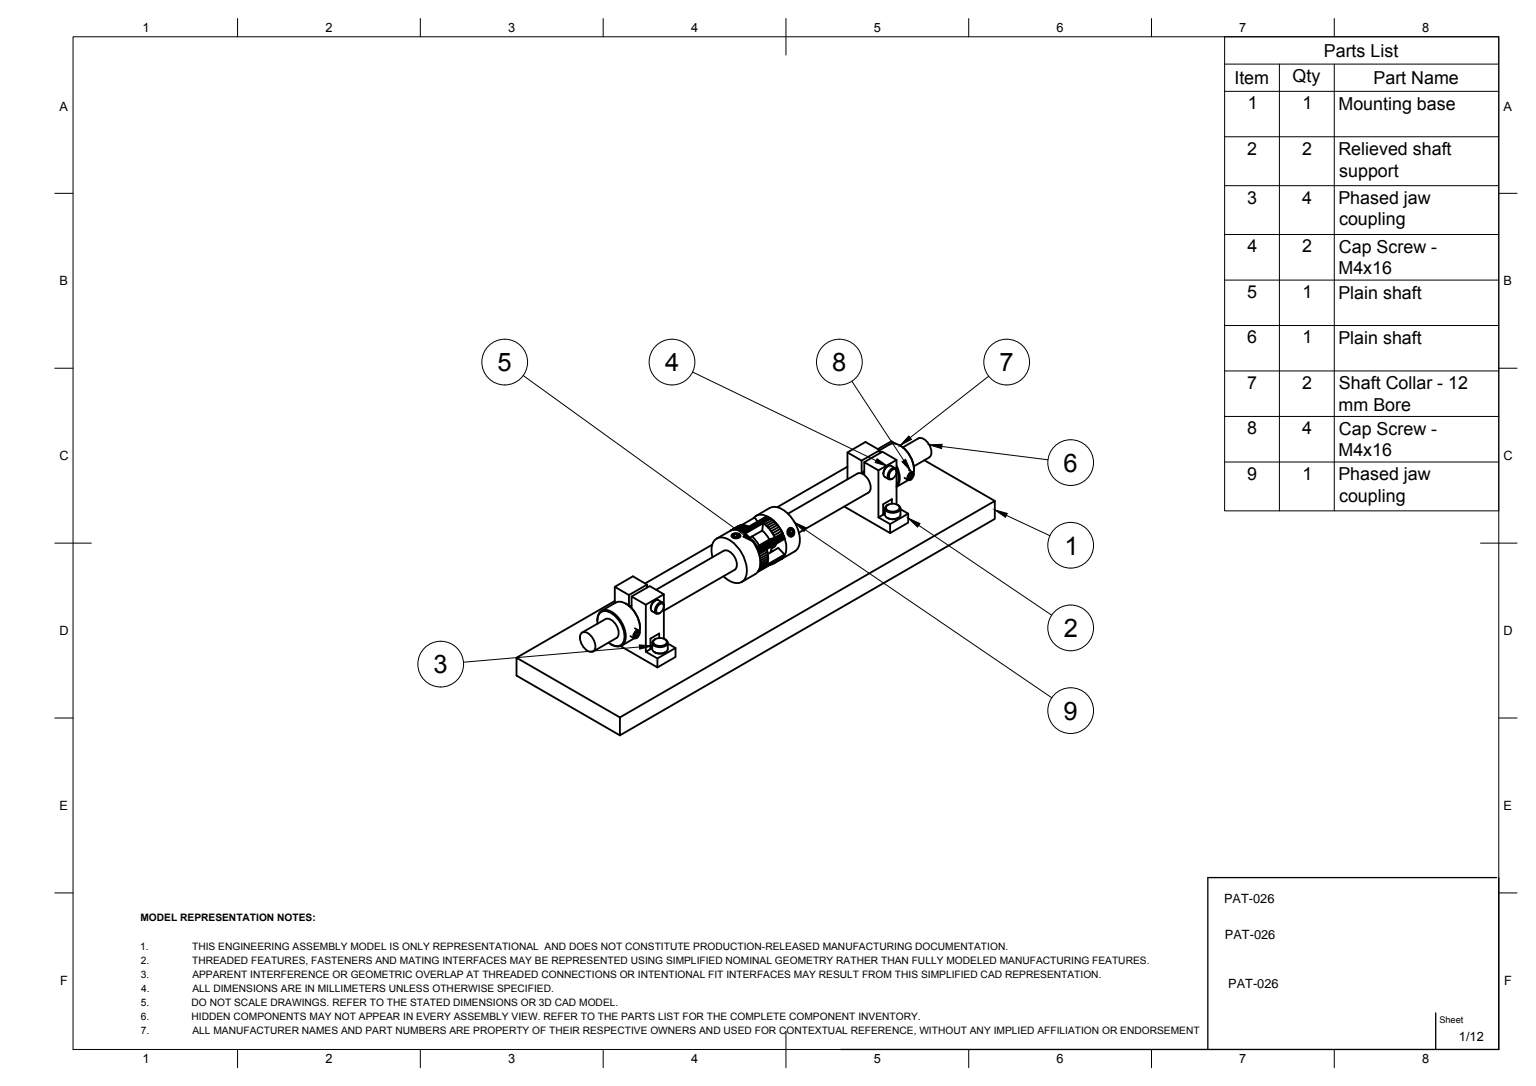
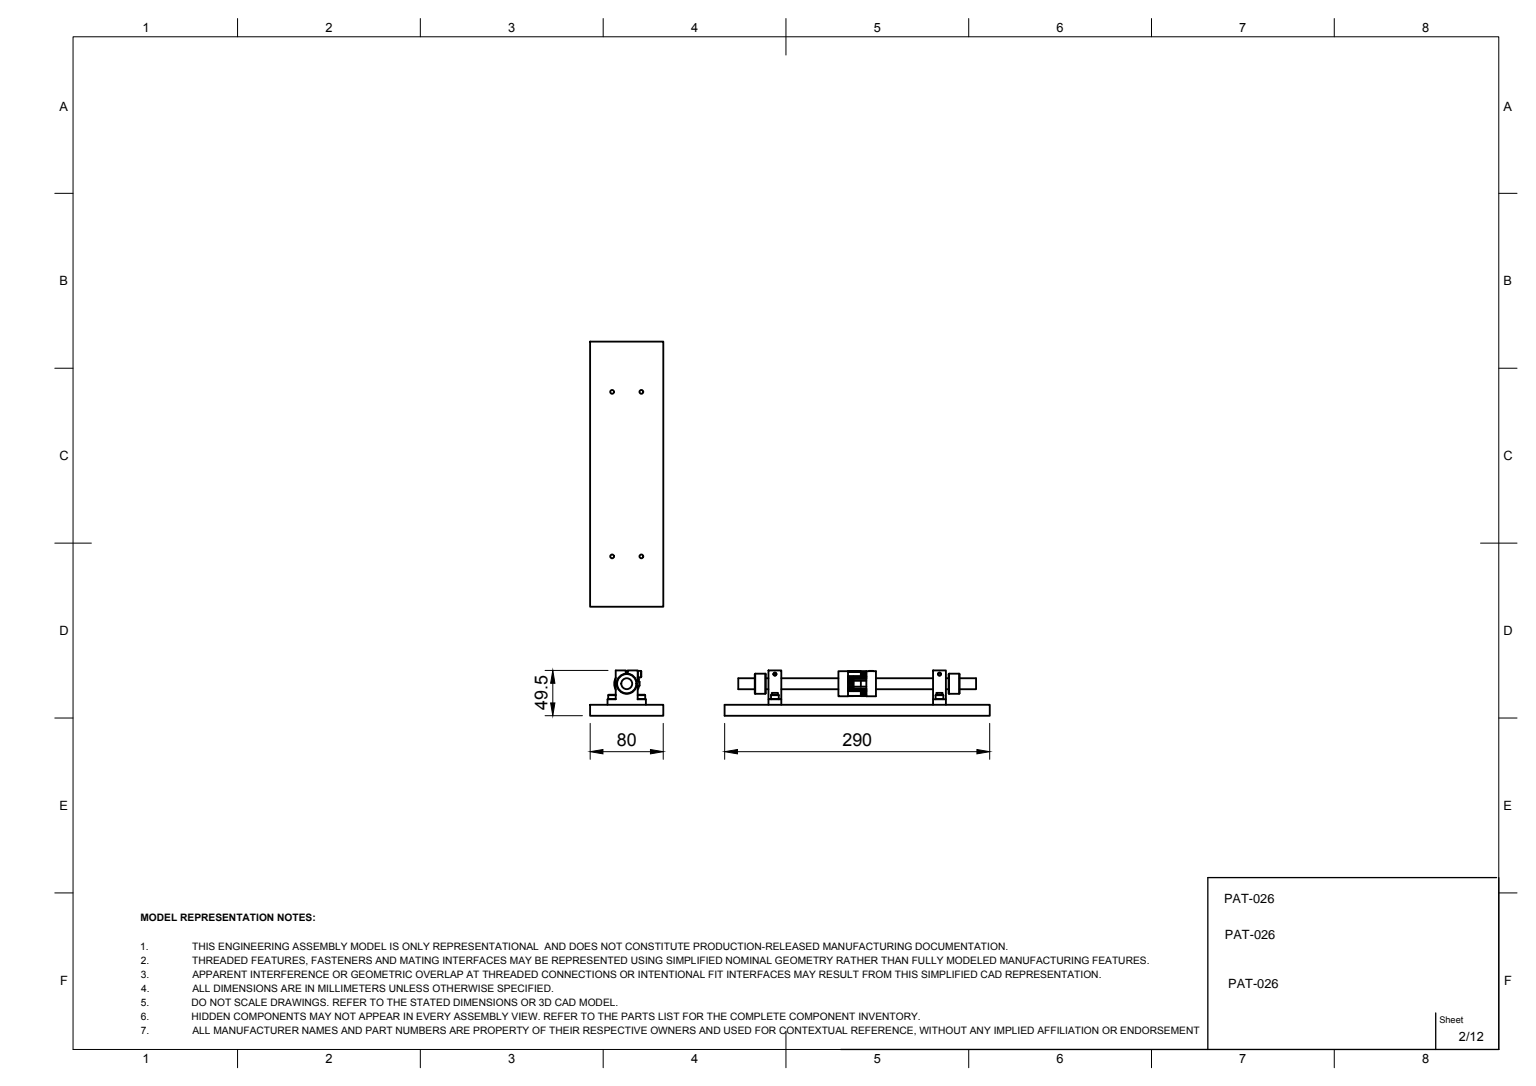
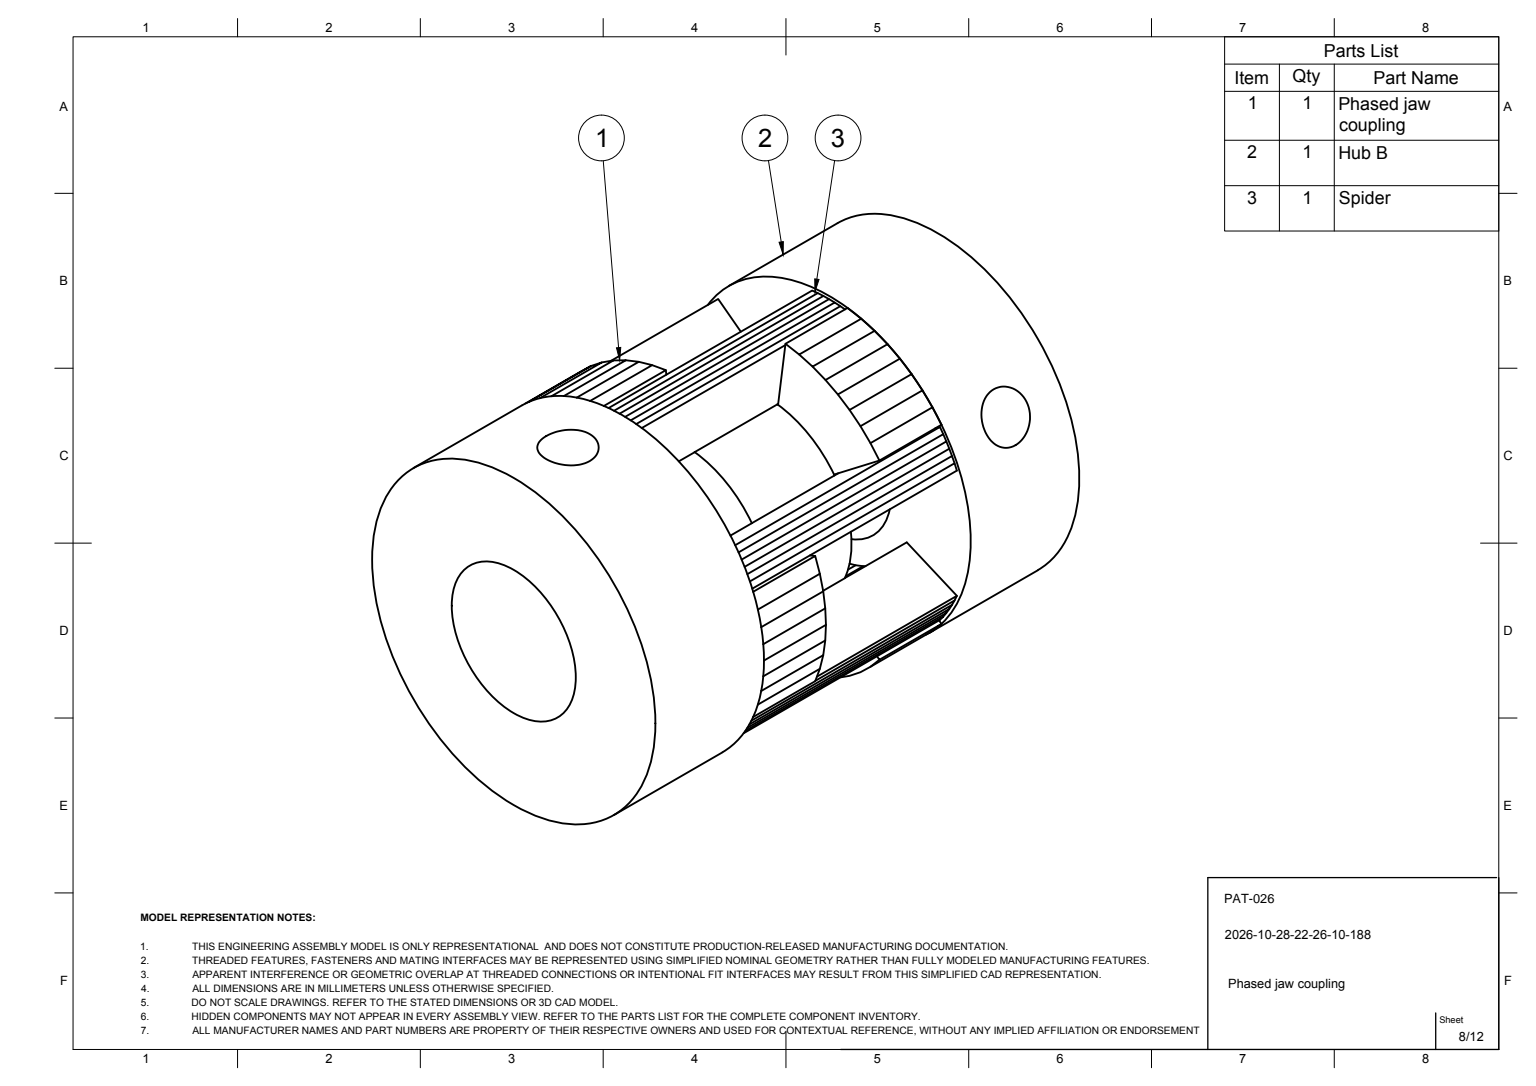
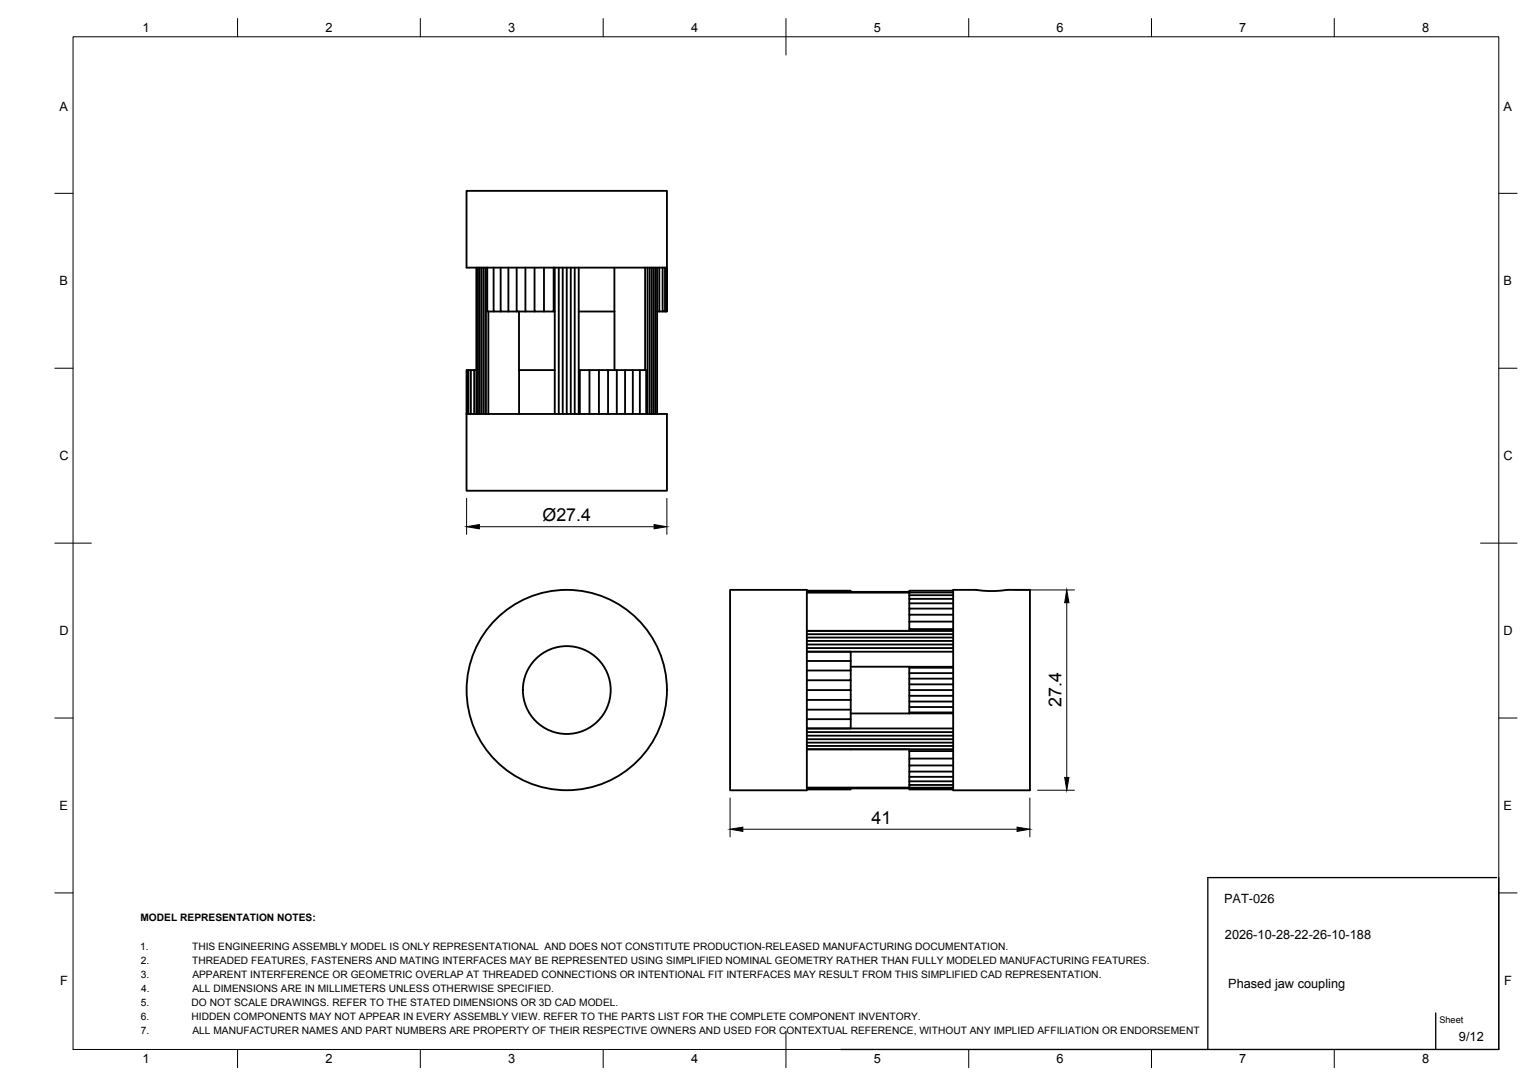
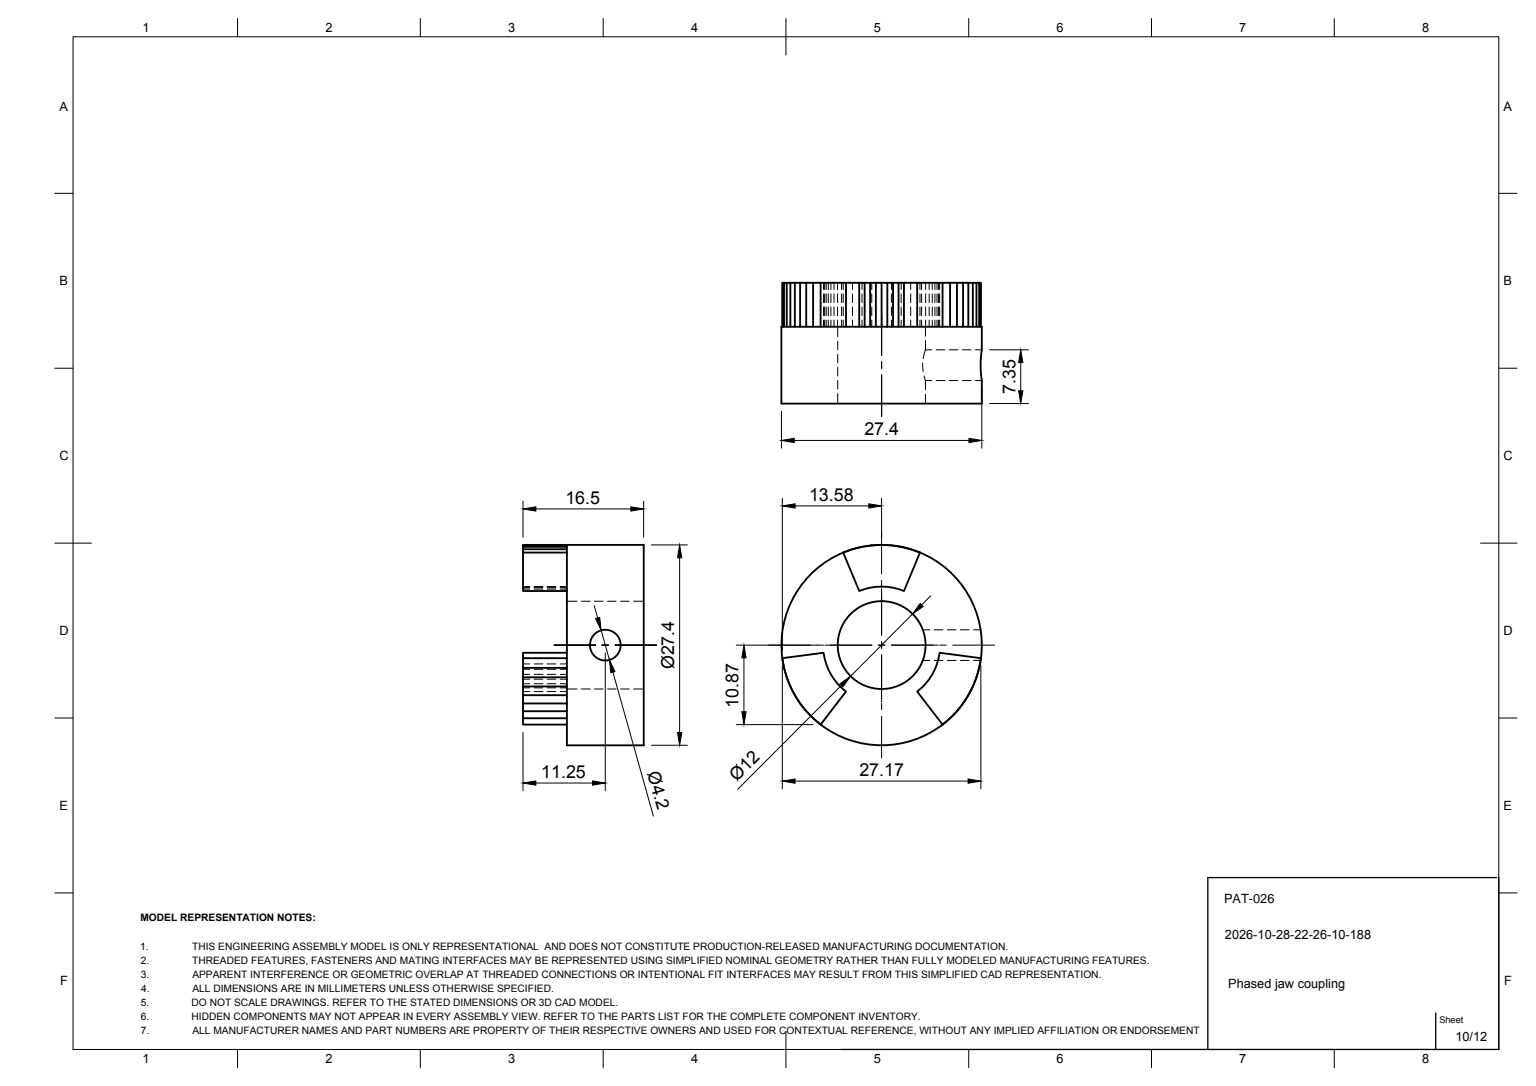
ISO-10303-21;
HEADER;
/* Generated by software containing ST-Developer
 * from STEP Tools, Inc. (www.steptools.com) 
 */

FILE_DESCRIPTION(
/* description */ ('PAT-026'),
/* implementation_level */ '2;1');

FILE_NAME(
/* name */ 'PAT-026',
/* time_stamp */ '2026-10-28T22:25:58-07:00',
/* author */ (''),
/* organization */ (''),
/* preprocessor_version */ 'ST-DEVELOPER v20.2',
/* originating_system */ 'Autodesk Translation Framework v15.17.0.0',
/* authorisation */ '');

FILE_SCHEMA (('AUTOMOTIVE_DESIGN { 1 0 10303 214 3 1 1 }'));
ENDSEC;

DATA;
#10=MECHANICAL_DESIGN_GEOMETRIC_PRESENTATION_REPRESENTATION('',(#141,#142,
#143,#144,#145,#146,#147,#148,#149,#150,#151),#12343);
#11=ITEM_DEFINED_TRANSFORMATION($,$,#7617,#8006);
#12=ITEM_DEFINED_TRANSFORMATION($,$,#7735,#8007);
#13=ITEM_DEFINED_TRANSFORMATION($,$,#7853,#8008);
#14=ITEM_DEFINED_TRANSFORMATION($,$,#7483,#8026);
#15=ITEM_DEFINED_TRANSFORMATION($,$,#7502,#8027);
#16=ITEM_DEFINED_TRANSFORMATION($,$,#7508,#8028);
#17=ITEM_DEFINED_TRANSFORMATION($,$,#7514,#8029);
#18=ITEM_DEFINED_TRANSFORMATION($,$,#7552,#8030);
#19=ITEM_DEFINED_TRANSFORMATION($,$,#7552,#8031);
#20=ITEM_DEFINED_TRANSFORMATION($,$,#7576,#8032);
#21=ITEM_DEFINED_TRANSFORMATION($,$,#7514,#8033);
#22=ITEM_DEFINED_TRANSFORMATION($,$,#7552,#8034);
#23=ITEM_DEFINED_TRANSFORMATION($,$,#7552,#8035);
#24=ITEM_DEFINED_TRANSFORMATION($,$,#7576,#8036);
#25=ITEM_DEFINED_TRANSFORMATION($,$,#7602,#8037);
#26=ITEM_DEFINED_TRANSFORMATION($,$,#8009,#8038);
#27=ITEM_DEFINED_TRANSFORMATION($,$,#7602,#8039);
#28=ITEM_DEFINED_TRANSFORMATION($,$,#8009,#8040);
#29=ITEM_DEFINED_TRANSFORMATION($,$,#7616,#8041);
#30=ITEM_DEFINED_TRANSFORMATION($,$,#8009,#8042);
#31=ITEM_DEFINED_TRANSFORMATION($,$,#8009,#8043);
#32=(
REPRESENTATION_RELATIONSHIP($,$,#12404,#12403)
REPRESENTATION_RELATIONSHIP_WITH_TRANSFORMATION(#11)
SHAPE_REPRESENTATION_RELATIONSHIP()
);
#33=(
REPRESENTATION_RELATIONSHIP($,$,#12405,#12403)
REPRESENTATION_RELATIONSHIP_WITH_TRANSFORMATION(#12)
SHAPE_REPRESENTATION_RELATIONSHIP()
);
#34=(
REPRESENTATION_RELATIONSHIP($,$,#12406,#12403)
REPRESENTATION_RELATIONSHIP_WITH_TRANSFORMATION(#13)
SHAPE_REPRESENTATION_RELATIONSHIP()
);
#35=(
REPRESENTATION_RELATIONSHIP($,$,#12396,#12395)
REPRESENTATION_RELATIONSHIP_WITH_TRANSFORMATION(#14)
SHAPE_REPRESENTATION_RELATIONSHIP()
);
#36=(
REPRESENTATION_RELATIONSHIP($,$,#12397,#12395)
REPRESENTATION_RELATIONSHIP_WITH_TRANSFORMATION(#15)
SHAPE_REPRESENTATION_RELATIONSHIP()
);
#37=(
REPRESENTATION_RELATIONSHIP($,$,#12398,#12395)
REPRESENTATION_RELATIONSHIP_WITH_TRANSFORMATION(#16)
SHAPE_REPRESENTATION_RELATIONSHIP()
);
#38=(
REPRESENTATION_RELATIONSHIP($,$,#12399,#12395)
REPRESENTATION_RELATIONSHIP_WITH_TRANSFORMATION(#17)
SHAPE_REPRESENTATION_RELATIONSHIP()
);
#39=(
REPRESENTATION_RELATIONSHIP($,$,#12400,#12395)
REPRESENTATION_RELATIONSHIP_WITH_TRANSFORMATION(#18)
SHAPE_REPRESENTATION_RELATIONSHIP()
);
#40=(
REPRESENTATION_RELATIONSHIP($,$,#12400,#12395)
REPRESENTATION_RELATIONSHIP_WITH_TRANSFORMATION(#19)
SHAPE_REPRESENTATION_RELATIONSHIP()
);
#41=(
REPRESENTATION_RELATIONSHIP($,$,#12401,#12395)
REPRESENTATION_RELATIONSHIP_WITH_TRANSFORMATION(#20)
SHAPE_REPRESENTATION_RELATIONSHIP()
);
#42=(
REPRESENTATION_RELATIONSHIP($,$,#12399,#12395)
REPRESENTATION_RELATIONSHIP_WITH_TRANSFORMATION(#21)
SHAPE_REPRESENTATION_RELATIONSHIP()
);
#43=(
REPRESENTATION_RELATIONSHIP($,$,#12400,#12395)
REPRESENTATION_RELATIONSHIP_WITH_TRANSFORMATION(#22)
SHAPE_REPRESENTATION_RELATIONSHIP()
);
#44=(
REPRESENTATION_RELATIONSHIP($,$,#12400,#12395)
REPRESENTATION_RELATIONSHIP_WITH_TRANSFORMATION(#23)
SHAPE_REPRESENTATION_RELATIONSHIP()
);
#45=(
REPRESENTATION_RELATIONSHIP($,$,#12401,#12395)
REPRESENTATION_RELATIONSHIP_WITH_TRANSFORMATION(#24)
SHAPE_REPRESENTATION_RELATIONSHIP()
);
#46=(
REPRESENTATION_RELATIONSHIP($,$,#12402,#12395)
REPRESENTATION_RELATIONSHIP_WITH_TRANSFORMATION(#25)
SHAPE_REPRESENTATION_RELATIONSHIP()
);
#47=(
REPRESENTATION_RELATIONSHIP($,$,#12407,#12395)
REPRESENTATION_RELATIONSHIP_WITH_TRANSFORMATION(#26)
SHAPE_REPRESENTATION_RELATIONSHIP()
);
#48=(
REPRESENTATION_RELATIONSHIP($,$,#12402,#12395)
REPRESENTATION_RELATIONSHIP_WITH_TRANSFORMATION(#27)
SHAPE_REPRESENTATION_RELATIONSHIP()
);
#49=(
REPRESENTATION_RELATIONSHIP($,$,#12407,#12395)
REPRESENTATION_RELATIONSHIP_WITH_TRANSFORMATION(#28)
SHAPE_REPRESENTATION_RELATIONSHIP()
);
#50=(
REPRESENTATION_RELATIONSHIP($,$,#12403,#12395)
REPRESENTATION_RELATIONSHIP_WITH_TRANSFORMATION(#29)
SHAPE_REPRESENTATION_RELATIONSHIP()
);
#51=(
REPRESENTATION_RELATIONSHIP($,$,#12407,#12395)
REPRESENTATION_RELATIONSHIP_WITH_TRANSFORMATION(#30)
SHAPE_REPRESENTATION_RELATIONSHIP()
);
#52=(
REPRESENTATION_RELATIONSHIP($,$,#12407,#12395)
REPRESENTATION_RELATIONSHIP_WITH_TRANSFORMATION(#31)
SHAPE_REPRESENTATION_RELATIONSHIP()
);
#53=CONTEXT_DEPENDENT_SHAPE_REPRESENTATION(#32,#12373);
#54=CONTEXT_DEPENDENT_SHAPE_REPRESENTATION(#33,#12374);
#55=CONTEXT_DEPENDENT_SHAPE_REPRESENTATION(#34,#12375);
#56=CONTEXT_DEPENDENT_SHAPE_REPRESENTATION(#35,#12377);
#57=CONTEXT_DEPENDENT_SHAPE_REPRESENTATION(#36,#12378);
#58=CONTEXT_DEPENDENT_SHAPE_REPRESENTATION(#37,#12379);
#59=CONTEXT_DEPENDENT_SHAPE_REPRESENTATION(#38,#12380);
#60=CONTEXT_DEPENDENT_SHAPE_REPRESENTATION(#39,#12381);
#61=CONTEXT_DEPENDENT_SHAPE_REPRESENTATION(#40,#12382);
#62=CONTEXT_DEPENDENT_SHAPE_REPRESENTATION(#41,#12383);
#63=CONTEXT_DEPENDENT_SHAPE_REPRESENTATION(#42,#12384);
#64=CONTEXT_DEPENDENT_SHAPE_REPRESENTATION(#43,#12385);
#65=CONTEXT_DEPENDENT_SHAPE_REPRESENTATION(#44,#12386);
#66=CONTEXT_DEPENDENT_SHAPE_REPRESENTATION(#45,#12387);
#67=CONTEXT_DEPENDENT_SHAPE_REPRESENTATION(#46,#12388);
#68=CONTEXT_DEPENDENT_SHAPE_REPRESENTATION(#47,#12389);
#69=CONTEXT_DEPENDENT_SHAPE_REPRESENTATION(#48,#12390);
#70=CONTEXT_DEPENDENT_SHAPE_REPRESENTATION(#49,#12391);
#71=CONTEXT_DEPENDENT_SHAPE_REPRESENTATION(#50,#12392);
#72=CONTEXT_DEPENDENT_SHAPE_REPRESENTATION(#51,#12393);
#73=CONTEXT_DEPENDENT_SHAPE_REPRESENTATION(#52,#12394);
#74=NEXT_ASSEMBLY_USAGE_OCCURRENCE('Hub A:1','Hub A:1','Hub A:1',#12417,
#12418,'Hub A:1');
#75=NEXT_ASSEMBLY_USAGE_OCCURRENCE('Hub B:1','Hub B:1','Hub B:1',#12417,
#12419,'Hub B:1');
#76=NEXT_ASSEMBLY_USAGE_OCCURRENCE('Spider:1','Spider:1','Spider:1',#12417,
#12420,'Spider:1');
#77=NEXT_ASSEMBLY_USAGE_OCCURRENCE('Mounting base:1','Mounting base:1',
'Mounting base:1',#12409,#12410,'Mounting base:1');
#78=NEXT_ASSEMBLY_USAGE_OCCURRENCE('Plain shaft:1','Plain shaft:1',
'Plain shaft:1',#12409,#12411,'Plain shaft:1');
#79=NEXT_ASSEMBLY_USAGE_OCCURRENCE('Plain shaft (1):1',
'Plain shaft (1):1','Plain shaft (1):1',#12409,#12412,
'Plain shaft (1):1');
#80=NEXT_ASSEMBLY_USAGE_OCCURRENCE('Relieved shaft support:1',
'Relieved shaft support:1','Relieved shaft support:1',#12409,#12413,
'Relieved shaft support:1');
#81=NEXT_ASSEMBLY_USAGE_OCCURRENCE('M5x14 Cap Screw:1',
'M5x14 Cap Screw:1','M5x14 Cap Screw:1',#12409,#12414,
'M5x14 Cap Screw:1');
#82=NEXT_ASSEMBLY_USAGE_OCCURRENCE('M5x14 Cap Screw:2',
'M5x14 Cap Screw:2','M5x14 Cap Screw:2',#12409,#12414,
'M5x14 Cap Screw:2');
#83=NEXT_ASSEMBLY_USAGE_OCCURRENCE('Cap Screw - M4x16:1',
'Cap Screw - M4x16:1','Cap Screw - M4x16:1',#12409,#12415,
'Cap Screw - M4x16:1');
#84=NEXT_ASSEMBLY_USAGE_OCCURRENCE('Relieved shaft support:2',
'Relieved shaft support:2','Relieved shaft support:2',#12409,#12413,
'Relieved shaft support:2');
#85=NEXT_ASSEMBLY_USAGE_OCCURRENCE('M5x14 Cap Screw:3',
'M5x14 Cap Screw:3','M5x14 Cap Screw:3',#12409,#12414,
'M5x14 Cap Screw:3');
#86=NEXT_ASSEMBLY_USAGE_OCCURRENCE('M5x14 Cap Screw:4',
'M5x14 Cap Screw:4','M5x14 Cap Screw:4',#12409,#12414,
'M5x14 Cap Screw:4');
#87=NEXT_ASSEMBLY_USAGE_OCCURRENCE('Cap Screw - M4x16:2',
'Cap Screw - M4x16:2','Cap Screw - M4x16:2',#12409,#12415,
'Cap Screw - M4x16:2');
#88=NEXT_ASSEMBLY_USAGE_OCCURRENCE('Shaft Collar - 12 mm Bore:1',
'Shaft Collar - 12 mm Bore:1','Shaft Collar - 12 mm Bore:1',#12409,#12416,
'Shaft Collar - 12 mm Bore:1');
#89=NEXT_ASSEMBLY_USAGE_OCCURRENCE('Socket Set Screw - M5x8:1',
'Socket Set Screw - M5x8:1','Socket Set Screw - M5x8:1',#12409,#12421,
'Socket Set Screw - M5x8:1');
#90=NEXT_ASSEMBLY_USAGE_OCCURRENCE('Shaft Collar - 12 mm Bore:2',
'Shaft Collar - 12 mm Bore:2','Shaft Collar - 12 mm Bore:2',#12409,#12416,
'Shaft Collar - 12 mm Bore:2');
#91=NEXT_ASSEMBLY_USAGE_OCCURRENCE('Socket Set Screw - M5x8:2',
'Socket Set Screw - M5x8:2','Socket Set Screw - M5x8:2',#12409,#12421,
'Socket Set Screw - M5x8:2');
#92=NEXT_ASSEMBLY_USAGE_OCCURRENCE('Phased jaw coupling:1',
'Phased jaw coupling:1','Phased jaw coupling:1',#12409,#12417,
'Phased jaw coupling:1');
#93=NEXT_ASSEMBLY_USAGE_OCCURRENCE('Socket Set Screw - M5x8:3',
'Socket Set Screw - M5x8:3','Socket Set Screw - M5x8:3',#12409,#12421,
'Socket Set Screw - M5x8:3');
#94=NEXT_ASSEMBLY_USAGE_OCCURRENCE('Socket Set Screw - M5x8:4',
'Socket Set Screw - M5x8:4','Socket Set Screw - M5x8:4',#12409,#12421,
'Socket Set Screw - M5x8:4');
#95=B_SPLINE_CURVE_WITH_KNOTS('',3,(#10378,#10379,#10380,#10381,#10382,
#10383,#10384,#10385,#10386,#10387,#10388,#10389,#10390,#10391,#10392,#10393,
#10394,#10395,#10396,#10397,#10398,#10399,#10400,#10401,#10402,#10403,#10404,
#10405,#10406,#10407,#10408,#10409,#10410,#10411),.UNSPECIFIED.,.T.,.F.,
(4,2,2,2,2,2,2,2,2,2,2,2,2,2,2,2,4),(0.,0.0805240527913139,0.161048105582628,
0.241524630728584,0.322001155874541,0.402477681020498,0.482954206166455,
0.563478258957768,0.644002311749082,0.724526364540396,0.80505041733171,
0.885526942477667,0.966003467623624,1.04647999276958,1.12695651791554,1.20748057070685,
1.28800462349816),.UNSPECIFIED.);
#96=B_SPLINE_CURVE_WITH_KNOTS('',3,(#10414,#10415,#10416,#10417,#10418,
#10419,#10420,#10421,#10422,#10423,#10424,#10425,#10426,#10427,#10428,#10429,
#10430,#10431,#10432,#10433,#10434,#10435,#10436,#10437,#10438,#10439,#10440,
#10441,#10442,#10443,#10444,#10445,#10446,#10447),.UNSPECIFIED.,.T.,.F.,
(4,2,2,2,2,2,2,2,2,2,2,2,2,2,2,2,4),(0.,0.0799614062161292,0.159922812432258,
0.239880387792505,0.319837963152752,0.399795538512999,0.479753113873245,
0.559714520089374,0.639675926305503,0.719637332521632,0.799598738737761,
0.879556314098008,0.959513889458255,1.0394714648185,1.11942904017875,1.19939044639488,
1.27935185261101),.UNSPECIFIED.);
#97=B_SPLINE_CURVE_WITH_KNOTS('',3,(#10475,#10476,#10477,#10478,#10479,
#10480,#10481,#10482,#10483,#10484,#10485,#10486,#10487,#10488,#10489,#10490,
#10491,#10492),.UNSPECIFIED.,.F.,.F.,(4,2,2,2,2,2,2,2,4),(0.,0.0798638474423531,
0.159727694884706,0.239545993340072,0.319364291795438,0.399182590250804,
0.47900088870617,0.558864736148523,0.638728583590876),.UNSPECIFIED.);
#98=B_SPLINE_CURVE_WITH_KNOTS('',3,(#10493,#10494,#10495,#10496,#10497,
#10498,#10499,#10500,#10501,#10502,#10503,#10504,#10505,#10506,#10507,#10508,
#10509,#10510),.UNSPECIFIED.,.F.,.F.,(4,2,2,2,2,2,2,2,4),(0.638728583590876,
0.718592431033229,0.798456278475582,0.878274576930948,0.958092875386314,
1.03791117384168,1.11772947229705,1.1975933197394,1.27745716718175),
 .UNSPECIFIED.);
#99=B_SPLINE_CURVE_WITH_KNOTS('',3,(#10513,#10514,#10515,#10516,#10517,
#10518,#10519,#10520,#10521,#10522,#10523,#10524,#10525,#10526,#10527,#10528,
#10529,#10530,#10531,#10532,#10533,#10534,#10535,#10536,#10537,#10538,#10539,
#10540,#10541,#10542,#10543,#10544,#10545,#10546),.UNSPECIFIED.,.T.,.F.,
(4,2,2,2,2,2,2,2,2,2,2,2,2,2,2,2,4),(0.,0.079239302416133,0.158478604832266,
0.237716399152057,0.316954193471848,0.39619198779164,0.475429782111431,
0.554669084527564,0.633908386943697,0.71314768935983,0.792386991775963,
0.871624786095754,0.950862580415545,1.03010037473534,1.10933816905513,1.18857747147126,
1.26781677388739),.UNSPECIFIED.);
#100=B_SPLINE_CURVE_WITH_KNOTS('',3,(#10943,#10944,#10945,#10946,#10947,
#10948,#10949,#10950,#10951,#10952,#10953,#10954,#10955,#10956,#10957,#10958,
#10959,#10960),.UNSPECIFIED.,.F.,.F.,(4,2,2,2,2,2,2,2,4),(0.,0.0798638474423531,
0.159727694884706,0.239545993340072,0.319364291795438,0.399182590250804,
0.47900088870617,0.558864736148523,0.638728583590876),.UNSPECIFIED.);
#101=B_SPLINE_CURVE_WITH_KNOTS('',3,(#10961,#10962,#10963,#10964,#10965,
#10966,#10967,#10968,#10969,#10970,#10971,#10972,#10973,#10974,#10975,#10976,
#10977,#10978),.UNSPECIFIED.,.F.,.F.,(4,2,2,2,2,2,2,2,4),(0.638728583590876,
0.718592431033229,0.798456278475583,0.878274576930949,0.958092875386314,
1.03791117384168,1.11772947229705,1.1975933197394,1.27745716718175),
 .UNSPECIFIED.);
#102=B_SPLINE_CURVE_WITH_KNOTS('',3,(#10982,#10983,#10984,#10985,#10986,
#10987,#10988,#10989,#10990,#10991,#10992,#10993,#10994,#10995,#10996,#10997,
#10998,#10999),.UNSPECIFIED.,.F.,.F.,(4,2,2,2,2,2,2,2,4),(0.,0.079239302416133,
0.158478604832266,0.237716399152057,0.316954193471848,0.39619198779164,
0.475429782111431,0.554669084527564,0.633908386943697),.UNSPECIFIED.);
#103=B_SPLINE_CURVE_WITH_KNOTS('',3,(#11000,#11001,#11002,#11003,#11004,
#11005,#11006,#11007,#11008,#11009,#11010,#11011,#11012,#11013,#11014,#11015,
#11016,#11017),.UNSPECIFIED.,.F.,.F.,(4,2,2,2,2,2,2,2,4),(0.633908386943697,
0.71314768935983,0.792386991775963,0.871624786095754,0.950862580415545,
1.03010037473534,1.10933816905513,1.18857747147126,1.26781677388739),
 .UNSPECIFIED.);
#104=CONICAL_SURFACE('',#7565,0.4,0.785398163397448);
#105=CONICAL_SURFACE('',#7569,0.41,0.785398163397448);
#106=CONICAL_SURFACE('',#7573,0.26,0.463647609000806);
#107=CONICAL_SURFACE('',#7579,0.325,0.785398163397448);
#108=CONICAL_SURFACE('',#7583,0.335,0.785398163397448);
#109=CONICAL_SURFACE('',#7587,0.21,0.463647609000806);
#110=CONICAL_SURFACE('',#7591,0.18,0.785398163397448);
#111=CONICAL_SURFACE('',#7607,1.075,0.785398163397448);
#112=CONICAL_SURFACE('',#7611,1.075,0.785398163397449);
#113=CONICAL_SURFACE('',#8019,0.235,0.785398163397448);
#114=CONICAL_SURFACE('',#8023,0.2125,0.785398163397448);
#115=ORIENTED_CLOSED_SHELL('',*,#7351,.F.);
#116=ORIENTED_CLOSED_SHELL('',*,#7354,.F.);
#117=BREP_WITH_VOIDS('Body1',#7352,(#115));
#118=BREP_WITH_VOIDS('Body1',#7353,(#116));
#119=SHAPE_REPRESENTATION_RELATIONSHIP('SRR','None',#12396,#130);
#120=SHAPE_REPRESENTATION_RELATIONSHIP('SRR','None',#12397,#131);
#121=SHAPE_REPRESENTATION_RELATIONSHIP('SRR','None',#12398,#132);
#122=SHAPE_REPRESENTATION_RELATIONSHIP('SRR','None',#12399,#133);
#123=SHAPE_REPRESENTATION_RELATIONSHIP('SRR','None',#12400,#134);
#124=SHAPE_REPRESENTATION_RELATIONSHIP('SRR','None',#12401,#135);
#125=SHAPE_REPRESENTATION_RELATIONSHIP('SRR','None',#12402,#136);
#126=SHAPE_REPRESENTATION_RELATIONSHIP('SRR','None',#12404,#137);
#127=SHAPE_REPRESENTATION_RELATIONSHIP('SRR','None',#12405,#138);
#128=SHAPE_REPRESENTATION_RELATIONSHIP('SRR','None',#12406,#139);
#129=SHAPE_REPRESENTATION_RELATIONSHIP('SRR','None',#12407,#140);
#130=ADVANCED_BREP_SHAPE_REPRESENTATION('',(#152),#12331);
#131=ADVANCED_BREP_SHAPE_REPRESENTATION('',(#153),#12332);
#132=ADVANCED_BREP_SHAPE_REPRESENTATION('',(#154),#12333);
#133=ADVANCED_BREP_SHAPE_REPRESENTATION('',(#155),#12334);
#134=ADVANCED_BREP_SHAPE_REPRESENTATION('',(#117),#12335);
#135=ADVANCED_BREP_SHAPE_REPRESENTATION('',(#118),#12336);
#136=ADVANCED_BREP_SHAPE_REPRESENTATION('',(#156),#12337);
#137=ADVANCED_BREP_SHAPE_REPRESENTATION('',(#157),#12339);
#138=ADVANCED_BREP_SHAPE_REPRESENTATION('',(#158),#12340);
#139=ADVANCED_BREP_SHAPE_REPRESENTATION('',(#159),#12341);
#140=ADVANCED_BREP_SHAPE_REPRESENTATION('',(#160),#12342);
#141=STYLED_ITEM('',(#12512),#152);
#142=STYLED_ITEM('',(#12533),#153);
#143=STYLED_ITEM('',(#12533),#154);
#144=STYLED_ITEM('',(#12533),#155);
#145=STYLED_ITEM('',(#12540),#117);
#146=STYLED_ITEM('',(#12540),#118);
#147=STYLED_ITEM('',(#12533),#156);
#148=STYLED_ITEM('',(#12526),#157);
#149=STYLED_ITEM('',(#12526),#158);
#150=STYLED_ITEM('',(#12526),#159);
#151=STYLED_ITEM('',(#12540),#160);
#152=MANIFOLD_SOLID_BREP('Body1',#7347);
#153=MANIFOLD_SOLID_BREP('Body1',#7348);
#154=MANIFOLD_SOLID_BREP('Body1',#7349);
#155=MANIFOLD_SOLID_BREP('Body1',#7350);
#156=MANIFOLD_SOLID_BREP('Body1',#7355);
#157=MANIFOLD_SOLID_BREP('Body1',#7356);
#158=MANIFOLD_SOLID_BREP('Body1',#7357);
#159=MANIFOLD_SOLID_BREP('Body1',#7358);
#160=MANIFOLD_SOLID_BREP('Body1',#7359);
#161=FACE_BOUND('',#965,.T.);
#162=FACE_BOUND('',#966,.T.);
#163=FACE_BOUND('',#967,.T.);
#164=FACE_BOUND('',#968,.T.);
#165=FACE_BOUND('',#970,.T.);
#166=FACE_BOUND('',#971,.T.);
#167=FACE_BOUND('',#972,.T.);
#168=FACE_BOUND('',#973,.T.);
#169=FACE_BOUND('',#985,.T.);
#170=FACE_BOUND('',#987,.T.);
#171=FACE_BOUND('',#989,.T.);
#172=FACE_BOUND('',#996,.T.);
#173=FACE_BOUND('',#999,.T.);
#174=FACE_BOUND('',#1000,.T.);
#175=FACE_BOUND('',#1003,.T.);
#176=FACE_BOUND('',#1006,.T.);
#177=FACE_BOUND('',#1009,.T.);
#178=FACE_BOUND('',#1012,.T.);
#179=FACE_BOUND('',#1027,.T.);
#180=FACE_BOUND('',#1035,.T.);
#181=FACE_BOUND('',#1050,.T.);
#182=FACE_BOUND('',#1053,.T.);
#183=FACE_BOUND('',#1056,.T.);
#184=FACE_BOUND('',#1058,.T.);
#185=FACE_BOUND('',#1061,.T.);
#186=FACE_BOUND('',#1090,.T.);
#187=FACE_BOUND('',#1146,.T.);
#188=FACE_BOUND('',#1148,.T.);
#189=FACE_BOUND('',#1151,.T.);
#190=FACE_BOUND('',#1178,.T.);
#191=FACE_BOUND('',#1236,.T.);
#192=FACE_BOUND('',#1238,.T.);
#193=FACE_BOUND('',#1387,.T.);
#194=PLANE('',#7496);
#195=PLANE('',#7497);
#196=PLANE('',#7498);
#197=PLANE('',#7499);
#198=PLANE('',#7500);
#199=PLANE('',#7501);
#200=PLANE('',#7506);
#201=PLANE('',#7507);
#202=PLANE('',#7512);
#203=PLANE('',#7513);
#204=PLANE('',#7515);
#205=PLANE('',#7522);
#206=PLANE('',#7523);
#207=PLANE('',#7525);
#208=PLANE('',#7527);
#209=PLANE('',#7541);
#210=PLANE('',#7542);
#211=PLANE('',#7543);
#212=PLANE('',#7544);
#213=PLANE('',#7545);
#214=PLANE('',#7546);
#215=PLANE('',#7547);
#216=PLANE('',#7548);
#217=PLANE('',#7549);
#218=PLANE('',#7550);
#219=PLANE('',#7551);
#220=PLANE('',#7553);
#221=PLANE('',#7554);
#222=PLANE('',#7555);
#223=PLANE('',#7556);
#224=PLANE('',#7557);
#225=PLANE('',#7558);
#226=PLANE('',#7559);
#227=PLANE('',#7560);
#228=PLANE('',#7561);
#229=PLANE('',#7563);
#230=PLANE('',#7571);
#231=PLANE('',#7577);
#232=PLANE('',#7585);
#233=PLANE('',#7593);
#234=PLANE('',#7594);
#235=PLANE('',#7595);
#236=PLANE('',#7596);
#237=PLANE('',#7597);
#238=PLANE('',#7598);
#239=PLANE('',#7599);
#240=PLANE('',#7600);
#241=PLANE('',#7601);
#242=PLANE('',#7604);
#243=PLANE('',#7613);
#244=PLANE('',#7622);
#245=PLANE('',#7623);
#246=PLANE('',#7624);
#247=PLANE('',#7625);
#248=PLANE('',#7626);
#249=PLANE('',#7627);
#250=PLANE('',#7628);
#251=PLANE('',#7629);
#252=PLANE('',#7630);
#253=PLANE('',#7631);
#254=PLANE('',#7632);
#255=PLANE('',#7633);
#256=PLANE('',#7634);
#257=PLANE('',#7635);
#258=PLANE('',#7636);
#259=PLANE('',#7637);
#260=PLANE('',#7638);
#261=PLANE('',#7639);
#262=PLANE('',#7640);
#263=PLANE('',#7641);
#264=PLANE('',#7643);
#265=PLANE('',#7645);
#266=PLANE('',#7647);
#267=PLANE('',#7649);
#268=PLANE('',#7651);
#269=PLANE('',#7653);
#270=PLANE('',#7655);
#271=PLANE('',#7657);
#272=PLANE('',#7662);
#273=PLANE('',#7663);
#274=PLANE('',#7664);
#275=PLANE('',#7665);
#276=PLANE('',#7666);
#277=PLANE('',#7667);
#278=PLANE('',#7668);
#279=PLANE('',#7669);
#280=PLANE('',#7670);
#281=PLANE('',#7671);
#282=PLANE('',#7672);
#283=PLANE('',#7673);
#284=PLANE('',#7674);
#285=PLANE('',#7675);
#286=PLANE('',#7676);
#287=PLANE('',#7677);
#288=PLANE('',#7678);
#289=PLANE('',#7679);
#290=PLANE('',#7680);
#291=PLANE('',#7681);
#292=PLANE('',#7683);
#293=PLANE('',#7685);
#294=PLANE('',#7687);
#295=PLANE('',#7689);
#296=PLANE('',#7691);
#297=PLANE('',#7693);
#298=PLANE('',#7695);
#299=PLANE('',#7697);
#300=PLANE('',#7698);
#301=PLANE('',#7699);
#302=PLANE('',#7700);
#303=PLANE('',#7701);
#304=PLANE('',#7702);
#305=PLANE('',#7703);
#306=PLANE('',#7704);
#307=PLANE('',#7705);
#308=PLANE('',#7706);
#309=PLANE('',#7707);
#310=PLANE('',#7708);
#311=PLANE('',#7709);
#312=PLANE('',#7710);
#313=PLANE('',#7711);
#314=PLANE('',#7712);
#315=PLANE('',#7713);
#316=PLANE('',#7714);
#317=PLANE('',#7715);
#318=PLANE('',#7716);
#319=PLANE('',#7718);
#320=PLANE('',#7720);
#321=PLANE('',#7722);
#322=PLANE('',#7724);
#323=PLANE('',#7726);
#324=PLANE('',#7728);
#325=PLANE('',#7730);
#326=PLANE('',#7734);
#327=PLANE('',#7740);
#328=PLANE('',#7741);
#329=PLANE('',#7742);
#330=PLANE('',#7743);
#331=PLANE('',#7744);
#332=PLANE('',#7745);
#333=PLANE('',#7746);
#334=PLANE('',#7747);
#335=PLANE('',#7748);
#336=PLANE('',#7749);
#337=PLANE('',#7750);
#338=PLANE('',#7751);
#339=PLANE('',#7752);
#340=PLANE('',#7753);
#341=PLANE('',#7754);
#342=PLANE('',#7755);
#343=PLANE('',#7756);
#344=PLANE('',#7757);
#345=PLANE('',#7758);
#346=PLANE('',#7759);
#347=PLANE('',#7761);
#348=PLANE('',#7763);
#349=PLANE('',#7765);
#350=PLANE('',#7767);
#351=PLANE('',#7769);
#352=PLANE('',#7771);
#353=PLANE('',#7776);
#354=PLANE('',#7778);
#355=PLANE('',#7780);
#356=PLANE('',#7781);
#357=PLANE('',#7782);
#358=PLANE('',#7783);
#359=PLANE('',#7784);
#360=PLANE('',#7785);
#361=PLANE('',#7786);
#362=PLANE('',#7787);
#363=PLANE('',#7788);
#364=PLANE('',#7789);
#365=PLANE('',#7790);
#366=PLANE('',#7791);
#367=PLANE('',#7792);
#368=PLANE('',#7793);
#369=PLANE('',#7794);
#370=PLANE('',#7795);
#371=PLANE('',#7796);
#372=PLANE('',#7797);
#373=PLANE('',#7798);
#374=PLANE('',#7799);
#375=PLANE('',#7801);
#376=PLANE('',#7803);
#377=PLANE('',#7805);
#378=PLANE('',#7807);
#379=PLANE('',#7809);
#380=PLANE('',#7811);
#381=PLANE('',#7813);
#382=PLANE('',#7815);
#383=PLANE('',#7816);
#384=PLANE('',#7817);
#385=PLANE('',#7818);
#386=PLANE('',#7819);
#387=PLANE('',#7820);
#388=PLANE('',#7821);
#389=PLANE('',#7822);
#390=PLANE('',#7823);
#391=PLANE('',#7824);
#392=PLANE('',#7825);
#393=PLANE('',#7826);
#394=PLANE('',#7827);
#395=PLANE('',#7828);
#396=PLANE('',#7829);
#397=PLANE('',#7830);
#398=PLANE('',#7831);
#399=PLANE('',#7832);
#400=PLANE('',#7833);
#401=PLANE('',#7834);
#402=PLANE('',#7836);
#403=PLANE('',#7838);
#404=PLANE('',#7840);
#405=PLANE('',#7842);
#406=PLANE('',#7844);
#407=PLANE('',#7846);
#408=PLANE('',#7848);
#409=PLANE('',#7852);
#410=PLANE('',#7854);
#411=PLANE('',#7873);
#412=PLANE('',#7874);
#413=PLANE('',#7875);
#414=PLANE('',#7876);
#415=PLANE('',#7877);
#416=PLANE('',#7878);
#417=PLANE('',#7879);
#418=PLANE('',#7880);
#419=PLANE('',#7881);
#420=PLANE('',#7882);
#421=PLANE('',#7883);
#422=PLANE('',#7884);
#423=PLANE('',#7885);
#424=PLANE('',#7886);
#425=PLANE('',#7887);
#426=PLANE('',#7888);
#427=PLANE('',#7889);
#428=PLANE('',#7890);
#429=PLANE('',#7891);
#430=PLANE('',#7892);
#431=PLANE('',#7893);
#432=PLANE('',#7894);
#433=PLANE('',#7895);
#434=PLANE('',#7896);
#435=PLANE('',#7897);
#436=PLANE('',#7898);
#437=PLANE('',#7899);
#438=PLANE('',#7900);
#439=PLANE('',#7901);
#440=PLANE('',#7902);
#441=PLANE('',#7903);
#442=PLANE('',#7904);
#443=PLANE('',#7905);
#444=PLANE('',#7906);
#445=PLANE('',#7907);
#446=PLANE('',#7908);
#447=PLANE('',#7909);
#448=PLANE('',#7910);
#449=PLANE('',#7911);
#450=PLANE('',#7912);
#451=PLANE('',#7913);
#452=PLANE('',#7914);
#453=PLANE('',#7915);
#454=PLANE('',#7916);
#455=PLANE('',#7917);
#456=PLANE('',#7918);
#457=PLANE('',#7919);
#458=PLANE('',#7920);
#459=PLANE('',#7921);
#460=PLANE('',#7922);
#461=PLANE('',#7923);
#462=PLANE('',#7924);
#463=PLANE('',#7925);
#464=PLANE('',#7926);
#465=PLANE('',#7927);
#466=PLANE('',#7928);
#467=PLANE('',#7929);
#468=PLANE('',#7930);
#469=PLANE('',#7931);
#470=PLANE('',#7932);
#471=PLANE('',#7933);
#472=PLANE('',#7934);
#473=PLANE('',#7935);
#474=PLANE('',#7936);
#475=PLANE('',#7937);
#476=PLANE('',#7938);
#477=PLANE('',#7939);
#478=PLANE('',#7940);
#479=PLANE('',#7941);
#480=PLANE('',#7942);
#481=PLANE('',#7943);
#482=PLANE('',#7944);
#483=PLANE('',#7945);
#484=PLANE('',#7946);
#485=PLANE('',#7947);
#486=PLANE('',#7948);
#487=PLANE('',#7949);
#488=PLANE('',#7950);
#489=PLANE('',#7951);
#490=PLANE('',#7952);
#491=PLANE('',#7953);
#492=PLANE('',#7954);
#493=PLANE('',#7955);
#494=PLANE('',#7956);
#495=PLANE('',#7957);
#496=PLANE('',#7958);
#497=PLANE('',#7959);
#498=PLANE('',#7960);
#499=PLANE('',#7961);
#500=PLANE('',#7962);
#501=PLANE('',#7963);
#502=PLANE('',#7964);
#503=PLANE('',#7965);
#504=PLANE('',#7966);
#505=PLANE('',#7967);
#506=PLANE('',#7968);
#507=PLANE('',#7969);
#508=PLANE('',#7970);
#509=PLANE('',#7971);
#510=PLANE('',#7972);
#511=PLANE('',#7973);
#512=PLANE('',#7974);
#513=PLANE('',#7975);
#514=PLANE('',#7976);
#515=PLANE('',#7977);
#516=PLANE('',#7978);
#517=PLANE('',#7979);
#518=PLANE('',#7980);
#519=PLANE('',#7981);
#520=PLANE('',#7982);
#521=PLANE('',#7983);
#522=PLANE('',#7984);
#523=PLANE('',#7985);
#524=PLANE('',#7986);
#525=PLANE('',#7987);
#526=PLANE('',#7988);
#527=PLANE('',#7989);
#528=PLANE('',#7990);
#529=PLANE('',#7991);
#530=PLANE('',#7992);
#531=PLANE('',#7993);
#532=PLANE('',#7994);
#533=PLANE('',#7995);
#534=PLANE('',#7996);
#535=PLANE('',#7997);
#536=PLANE('',#7998);
#537=PLANE('',#7999);
#538=PLANE('',#8000);
#539=PLANE('',#8001);
#540=PLANE('',#8002);
#541=PLANE('',#8003);
#542=PLANE('',#8004);
#543=PLANE('',#8005);
#544=PLANE('',#8010);
#545=PLANE('',#8011);
#546=PLANE('',#8012);
#547=PLANE('',#8013);
#548=PLANE('',#8014);
#549=PLANE('',#8015);
#550=PLANE('',#8016);
#551=PLANE('',#8017);
#552=PLANE('',#8025);
#553=FACE_OUTER_BOUND('',#956,.T.);
#554=FACE_OUTER_BOUND('',#957,.T.);
#555=FACE_OUTER_BOUND('',#958,.T.);
#556=FACE_OUTER_BOUND('',#959,.T.);
#557=FACE_OUTER_BOUND('',#960,.T.);
#558=FACE_OUTER_BOUND('',#961,.T.);
#559=FACE_OUTER_BOUND('',#962,.T.);
#560=FACE_OUTER_BOUND('',#963,.T.);
#561=FACE_OUTER_BOUND('',#964,.T.);
#562=FACE_OUTER_BOUND('',#969,.T.);
#563=FACE_OUTER_BOUND('',#974,.T.);
#564=FACE_OUTER_BOUND('',#975,.T.);
#565=FACE_OUTER_BOUND('',#976,.T.);
#566=FACE_OUTER_BOUND('',#977,.T.);
#567=FACE_OUTER_BOUND('',#978,.T.);
#568=FACE_OUTER_BOUND('',#979,.T.);
#569=FACE_OUTER_BOUND('',#980,.T.);
#570=FACE_OUTER_BOUND('',#981,.T.);
#571=FACE_OUTER_BOUND('',#982,.T.);
#572=FACE_OUTER_BOUND('',#983,.T.);
#573=FACE_OUTER_BOUND('',#984,.T.);
#574=FACE_OUTER_BOUND('',#986,.T.);
#575=FACE_OUTER_BOUND('',#988,.T.);
#576=FACE_OUTER_BOUND('',#990,.T.);
#577=FACE_OUTER_BOUND('',#991,.T.);
#578=FACE_OUTER_BOUND('',#992,.T.);
#579=FACE_OUTER_BOUND('',#993,.T.);
#580=FACE_OUTER_BOUND('',#994,.T.);
#581=FACE_OUTER_BOUND('',#995,.T.);
#582=FACE_OUTER_BOUND('',#997,.T.);
#583=FACE_OUTER_BOUND('',#998,.T.);
#584=FACE_OUTER_BOUND('',#1001,.T.);
#585=FACE_OUTER_BOUND('',#1002,.T.);
#586=FACE_OUTER_BOUND('',#1004,.T.);
#587=FACE_OUTER_BOUND('',#1005,.T.);
#588=FACE_OUTER_BOUND('',#1007,.T.);
#589=FACE_OUTER_BOUND('',#1008,.T.);
#590=FACE_OUTER_BOUND('',#1010,.T.);
#591=FACE_OUTER_BOUND('',#1011,.T.);
#592=FACE_OUTER_BOUND('',#1013,.T.);
#593=FACE_OUTER_BOUND('',#1014,.T.);
#594=FACE_OUTER_BOUND('',#1015,.T.);
#595=FACE_OUTER_BOUND('',#1016,.T.);
#596=FACE_OUTER_BOUND('',#1017,.T.);
#597=FACE_OUTER_BOUND('',#1018,.T.);
#598=FACE_OUTER_BOUND('',#1019,.T.);
#599=FACE_OUTER_BOUND('',#1020,.T.);
#600=FACE_OUTER_BOUND('',#1021,.T.);
#601=FACE_OUTER_BOUND('',#1022,.T.);
#602=FACE_OUTER_BOUND('',#1023,.T.);
#603=FACE_OUTER_BOUND('',#1024,.T.);
#604=FACE_OUTER_BOUND('',#1025,.T.);
#605=FACE_OUTER_BOUND('',#1026,.T.);
#606=FACE_OUTER_BOUND('',#1028,.T.);
#607=FACE_OUTER_BOUND('',#1029,.T.);
#608=FACE_OUTER_BOUND('',#1030,.T.);
#609=FACE_OUTER_BOUND('',#1031,.T.);
#610=FACE_OUTER_BOUND('',#1032,.T.);
#611=FACE_OUTER_BOUND('',#1033,.T.);
#612=FACE_OUTER_BOUND('',#1034,.T.);
#613=FACE_OUTER_BOUND('',#1036,.T.);
#614=FACE_OUTER_BOUND('',#1037,.T.);
#615=FACE_OUTER_BOUND('',#1038,.T.);
#616=FACE_OUTER_BOUND('',#1039,.T.);
#617=FACE_OUTER_BOUND('',#1040,.T.);
#618=FACE_OUTER_BOUND('',#1041,.T.);
#619=FACE_OUTER_BOUND('',#1042,.T.);
#620=FACE_OUTER_BOUND('',#1043,.T.);
#621=FACE_OUTER_BOUND('',#1044,.T.);
#622=FACE_OUTER_BOUND('',#1045,.T.);
#623=FACE_OUTER_BOUND('',#1046,.T.);
#624=FACE_OUTER_BOUND('',#1047,.T.);
#625=FACE_OUTER_BOUND('',#1048,.T.);
#626=FACE_OUTER_BOUND('',#1049,.T.);
#627=FACE_OUTER_BOUND('',#1051,.T.);
#628=FACE_OUTER_BOUND('',#1052,.T.);
#629=FACE_OUTER_BOUND('',#1054,.T.);
#630=FACE_OUTER_BOUND('',#1055,.T.);
#631=FACE_OUTER_BOUND('',#1057,.T.);
#632=FACE_OUTER_BOUND('',#1059,.T.);
#633=FACE_OUTER_BOUND('',#1060,.T.);
#634=FACE_OUTER_BOUND('',#1062,.T.);
#635=FACE_OUTER_BOUND('',#1063,.T.);
#636=FACE_OUTER_BOUND('',#1064,.T.);
#637=FACE_OUTER_BOUND('',#1065,.T.);
#638=FACE_OUTER_BOUND('',#1066,.T.);
#639=FACE_OUTER_BOUND('',#1067,.T.);
#640=FACE_OUTER_BOUND('',#1068,.T.);
#641=FACE_OUTER_BOUND('',#1069,.T.);
#642=FACE_OUTER_BOUND('',#1070,.T.);
#643=FACE_OUTER_BOUND('',#1071,.T.);
#644=FACE_OUTER_BOUND('',#1072,.T.);
#645=FACE_OUTER_BOUND('',#1073,.T.);
#646=FACE_OUTER_BOUND('',#1074,.T.);
#647=FACE_OUTER_BOUND('',#1075,.T.);
#648=FACE_OUTER_BOUND('',#1076,.T.);
#649=FACE_OUTER_BOUND('',#1077,.T.);
#650=FACE_OUTER_BOUND('',#1078,.T.);
#651=FACE_OUTER_BOUND('',#1079,.T.);
#652=FACE_OUTER_BOUND('',#1080,.T.);
#653=FACE_OUTER_BOUND('',#1081,.T.);
#654=FACE_OUTER_BOUND('',#1082,.T.);
#655=FACE_OUTER_BOUND('',#1083,.T.);
#656=FACE_OUTER_BOUND('',#1084,.T.);
#657=FACE_OUTER_BOUND('',#1085,.T.);
#658=FACE_OUTER_BOUND('',#1086,.T.);
#659=FACE_OUTER_BOUND('',#1087,.T.);
#660=FACE_OUTER_BOUND('',#1088,.T.);
#661=FACE_OUTER_BOUND('',#1089,.T.);
#662=FACE_OUTER_BOUND('',#1091,.T.);
#663=FACE_OUTER_BOUND('',#1092,.T.);
#664=FACE_OUTER_BOUND('',#1093,.T.);
#665=FACE_OUTER_BOUND('',#1094,.T.);
#666=FACE_OUTER_BOUND('',#1095,.T.);
#667=FACE_OUTER_BOUND('',#1096,.T.);
#668=FACE_OUTER_BOUND('',#1097,.T.);
#669=FACE_OUTER_BOUND('',#1098,.T.);
#670=FACE_OUTER_BOUND('',#1099,.T.);
#671=FACE_OUTER_BOUND('',#1100,.T.);
#672=FACE_OUTER_BOUND('',#1101,.T.);
#673=FACE_OUTER_BOUND('',#1102,.T.);
#674=FACE_OUTER_BOUND('',#1103,.T.);
#675=FACE_OUTER_BOUND('',#1104,.T.);
#676=FACE_OUTER_BOUND('',#1105,.T.);
#677=FACE_OUTER_BOUND('',#1106,.T.);
#678=FACE_OUTER_BOUND('',#1107,.T.);
#679=FACE_OUTER_BOUND('',#1108,.T.);
#680=FACE_OUTER_BOUND('',#1109,.T.);
#681=FACE_OUTER_BOUND('',#1110,.T.);
#682=FACE_OUTER_BOUND('',#1111,.T.);
#683=FACE_OUTER_BOUND('',#1112,.T.);
#684=FACE_OUTER_BOUND('',#1113,.T.);
#685=FACE_OUTER_BOUND('',#1114,.T.);
#686=FACE_OUTER_BOUND('',#1115,.T.);
#687=FACE_OUTER_BOUND('',#1116,.T.);
#688=FACE_OUTER_BOUND('',#1117,.T.);
#689=FACE_OUTER_BOUND('',#1118,.T.);
#690=FACE_OUTER_BOUND('',#1119,.T.);
#691=FACE_OUTER_BOUND('',#1120,.T.);
#692=FACE_OUTER_BOUND('',#1121,.T.);
#693=FACE_OUTER_BOUND('',#1122,.T.);
#694=FACE_OUTER_BOUND('',#1123,.T.);
#695=FACE_OUTER_BOUND('',#1124,.T.);
#696=FACE_OUTER_BOUND('',#1125,.T.);
#697=FACE_OUTER_BOUND('',#1126,.T.);
#698=FACE_OUTER_BOUND('',#1127,.T.);
#699=FACE_OUTER_BOUND('',#1128,.T.);
#700=FACE_OUTER_BOUND('',#1129,.T.);
#701=FACE_OUTER_BOUND('',#1130,.T.);
#702=FACE_OUTER_BOUND('',#1131,.T.);
#703=FACE_OUTER_BOUND('',#1132,.T.);
#704=FACE_OUTER_BOUND('',#1133,.T.);
#705=FACE_OUTER_BOUND('',#1134,.T.);
#706=FACE_OUTER_BOUND('',#1135,.T.);
#707=FACE_OUTER_BOUND('',#1136,.T.);
#708=FACE_OUTER_BOUND('',#1137,.T.);
#709=FACE_OUTER_BOUND('',#1138,.T.);
#710=FACE_OUTER_BOUND('',#1139,.T.);
#711=FACE_OUTER_BOUND('',#1140,.T.);
#712=FACE_OUTER_BOUND('',#1141,.T.);
#713=FACE_OUTER_BOUND('',#1142,.T.);
#714=FACE_OUTER_BOUND('',#1143,.T.);
#715=FACE_OUTER_BOUND('',#1144,.T.);
#716=FACE_OUTER_BOUND('',#1145,.T.);
#717=FACE_OUTER_BOUND('',#1147,.T.);
#718=FACE_OUTER_BOUND('',#1149,.T.);
#719=FACE_OUTER_BOUND('',#1150,.T.);
#720=FACE_OUTER_BOUND('',#1152,.T.);
#721=FACE_OUTER_BOUND('',#1153,.T.);
#722=FACE_OUTER_BOUND('',#1154,.T.);
#723=FACE_OUTER_BOUND('',#1155,.T.);
#724=FACE_OUTER_BOUND('',#1156,.T.);
#725=FACE_OUTER_BOUND('',#1157,.T.);
#726=FACE_OUTER_BOUND('',#1158,.T.);
#727=FACE_OUTER_BOUND('',#1159,.T.);
#728=FACE_OUTER_BOUND('',#1160,.T.);
#729=FACE_OUTER_BOUND('',#1161,.T.);
#730=FACE_OUTER_BOUND('',#1162,.T.);
#731=FACE_OUTER_BOUND('',#1163,.T.);
#732=FACE_OUTER_BOUND('',#1164,.T.);
#733=FACE_OUTER_BOUND('',#1165,.T.);
#734=FACE_OUTER_BOUND('',#1166,.T.);
#735=FACE_OUTER_BOUND('',#1167,.T.);
#736=FACE_OUTER_BOUND('',#1168,.T.);
#737=FACE_OUTER_BOUND('',#1169,.T.);
#738=FACE_OUTER_BOUND('',#1170,.T.);
#739=FACE_OUTER_BOUND('',#1171,.T.);
#740=FACE_OUTER_BOUND('',#1172,.T.);
#741=FACE_OUTER_BOUND('',#1173,.T.);
#742=FACE_OUTER_BOUND('',#1174,.T.);
#743=FACE_OUTER_BOUND('',#1175,.T.);
#744=FACE_OUTER_BOUND('',#1176,.T.);
#745=FACE_OUTER_BOUND('',#1177,.T.);
#746=FACE_OUTER_BOUND('',#1179,.T.);
#747=FACE_OUTER_BOUND('',#1180,.T.);
#748=FACE_OUTER_BOUND('',#1181,.T.);
#749=FACE_OUTER_BOUND('',#1182,.T.);
#750=FACE_OUTER_BOUND('',#1183,.T.);
#751=FACE_OUTER_BOUND('',#1184,.T.);
#752=FACE_OUTER_BOUND('',#1185,.T.);
#753=FACE_OUTER_BOUND('',#1186,.T.);
#754=FACE_OUTER_BOUND('',#1187,.T.);
#755=FACE_OUTER_BOUND('',#1188,.T.);
#756=FACE_OUTER_BOUND('',#1189,.T.);
#757=FACE_OUTER_BOUND('',#1190,.T.);
#758=FACE_OUTER_BOUND('',#1191,.T.);
#759=FACE_OUTER_BOUND('',#1192,.T.);
#760=FACE_OUTER_BOUND('',#1193,.T.);
#761=FACE_OUTER_BOUND('',#1194,.T.);
#762=FACE_OUTER_BOUND('',#1195,.T.);
#763=FACE_OUTER_BOUND('',#1196,.T.);
#764=FACE_OUTER_BOUND('',#1197,.T.);
#765=FACE_OUTER_BOUND('',#1198,.T.);
#766=FACE_OUTER_BOUND('',#1199,.T.);
#767=FACE_OUTER_BOUND('',#1200,.T.);
#768=FACE_OUTER_BOUND('',#1201,.T.);
#769=FACE_OUTER_BOUND('',#1202,.T.);
#770=FACE_OUTER_BOUND('',#1203,.T.);
#771=FACE_OUTER_BOUND('',#1204,.T.);
#772=FACE_OUTER_BOUND('',#1205,.T.);
#773=FACE_OUTER_BOUND('',#1206,.T.);
#774=FACE_OUTER_BOUND('',#1207,.T.);
#775=FACE_OUTER_BOUND('',#1208,.T.);
#776=FACE_OUTER_BOUND('',#1209,.T.);
#777=FACE_OUTER_BOUND('',#1210,.T.);
#778=FACE_OUTER_BOUND('',#1211,.T.);
#779=FACE_OUTER_BOUND('',#1212,.T.);
#780=FACE_OUTER_BOUND('',#1213,.T.);
#781=FACE_OUTER_BOUND('',#1214,.T.);
#782=FACE_OUTER_BOUND('',#1215,.T.);
#783=FACE_OUTER_BOUND('',#1216,.T.);
#784=FACE_OUTER_BOUND('',#1217,.T.);
#785=FACE_OUTER_BOUND('',#1218,.T.);
#786=FACE_OUTER_BOUND('',#1219,.T.);
#787=FACE_OUTER_BOUND('',#1220,.T.);
#788=FACE_OUTER_BOUND('',#1221,.T.);
#789=FACE_OUTER_BOUND('',#1222,.T.);
#790=FACE_OUTER_BOUND('',#1223,.T.);
#791=FACE_OUTER_BOUND('',#1224,.T.);
#792=FACE_OUTER_BOUND('',#1225,.T.);
#793=FACE_OUTER_BOUND('',#1226,.T.);
#794=FACE_OUTER_BOUND('',#1227,.T.);
#795=FACE_OUTER_BOUND('',#1228,.T.);
#796=FACE_OUTER_BOUND('',#1229,.T.);
#797=FACE_OUTER_BOUND('',#1230,.T.);
#798=FACE_OUTER_BOUND('',#1231,.T.);
#799=FACE_OUTER_BOUND('',#1232,.T.);
#800=FACE_OUTER_BOUND('',#1233,.T.);
#801=FACE_OUTER_BOUND('',#1234,.T.);
#802=FACE_OUTER_BOUND('',#1235,.T.);
#803=FACE_OUTER_BOUND('',#1237,.T.);
#804=FACE_OUTER_BOUND('',#1239,.T.);
#805=FACE_OUTER_BOUND('',#1240,.T.);
#806=FACE_OUTER_BOUND('',#1241,.T.);
#807=FACE_OUTER_BOUND('',#1242,.T.);
#808=FACE_OUTER_BOUND('',#1243,.T.);
#809=FACE_OUTER_BOUND('',#1244,.T.);
#810=FACE_OUTER_BOUND('',#1245,.T.);
#811=FACE_OUTER_BOUND('',#1246,.T.);
#812=FACE_OUTER_BOUND('',#1247,.T.);
#813=FACE_OUTER_BOUND('',#1248,.T.);
#814=FACE_OUTER_BOUND('',#1249,.T.);
#815=FACE_OUTER_BOUND('',#1250,.T.);
#816=FACE_OUTER_BOUND('',#1251,.T.);
#817=FACE_OUTER_BOUND('',#1252,.T.);
#818=FACE_OUTER_BOUND('',#1253,.T.);
#819=FACE_OUTER_BOUND('',#1254,.T.);
#820=FACE_OUTER_BOUND('',#1255,.T.);
#821=FACE_OUTER_BOUND('',#1256,.T.);
#822=FACE_OUTER_BOUND('',#1257,.T.);
#823=FACE_OUTER_BOUND('',#1258,.T.);
#824=FACE_OUTER_BOUND('',#1259,.T.);
#825=FACE_OUTER_BOUND('',#1260,.T.);
#826=FACE_OUTER_BOUND('',#1261,.T.);
#827=FACE_OUTER_BOUND('',#1262,.T.);
#828=FACE_OUTER_BOUND('',#1263,.T.);
#829=FACE_OUTER_BOUND('',#1264,.T.);
#830=FACE_OUTER_BOUND('',#1265,.T.);
#831=FACE_OUTER_BOUND('',#1266,.T.);
#832=FACE_OUTER_BOUND('',#1267,.T.);
#833=FACE_OUTER_BOUND('',#1268,.T.);
#834=FACE_OUTER_BOUND('',#1269,.T.);
#835=FACE_OUTER_BOUND('',#1270,.T.);
#836=FACE_OUTER_BOUND('',#1271,.T.);
#837=FACE_OUTER_BOUND('',#1272,.T.);
#838=FACE_OUTER_BOUND('',#1273,.T.);
#839=FACE_OUTER_BOUND('',#1274,.T.);
#840=FACE_OUTER_BOUND('',#1275,.T.);
#841=FACE_OUTER_BOUND('',#1276,.T.);
#842=FACE_OUTER_BOUND('',#1277,.T.);
#843=FACE_OUTER_BOUND('',#1278,.T.);
#844=FACE_OUTER_BOUND('',#1279,.T.);
#845=FACE_OUTER_BOUND('',#1280,.T.);
#846=FACE_OUTER_BOUND('',#1281,.T.);
#847=FACE_OUTER_BOUND('',#1282,.T.);
#848=FACE_OUTER_BOUND('',#1283,.T.);
#849=FACE_OUTER_BOUND('',#1284,.T.);
#850=FACE_OUTER_BOUND('',#1285,.T.);
#851=FACE_OUTER_BOUND('',#1286,.T.);
#852=FACE_OUTER_BOUND('',#1287,.T.);
#853=FACE_OUTER_BOUND('',#1288,.T.);
#854=FACE_OUTER_BOUND('',#1289,.T.);
#855=FACE_OUTER_BOUND('',#1290,.T.);
#856=FACE_OUTER_BOUND('',#1291,.T.);
#857=FACE_OUTER_BOUND('',#1292,.T.);
#858=FACE_OUTER_BOUND('',#1293,.T.);
#859=FACE_OUTER_BOUND('',#1294,.T.);
#860=FACE_OUTER_BOUND('',#1295,.T.);
#861=FACE_OUTER_BOUND('',#1296,.T.);
#862=FACE_OUTER_BOUND('',#1297,.T.);
#863=FACE_OUTER_BOUND('',#1298,.T.);
#864=FACE_OUTER_BOUND('',#1299,.T.);
#865=FACE_OUTER_BOUND('',#1300,.T.);
#866=FACE_OUTER_BOUND('',#1301,.T.);
#867=FACE_OUTER_BOUND('',#1302,.T.);
#868=FACE_OUTER_BOUND('',#1303,.T.);
#869=FACE_OUTER_BOUND('',#1304,.T.);
#870=FACE_OUTER_BOUND('',#1305,.T.);
#871=FACE_OUTER_BOUND('',#1306,.T.);
#872=FACE_OUTER_BOUND('',#1307,.T.);
#873=FACE_OUTER_BOUND('',#1308,.T.);
#874=FACE_OUTER_BOUND('',#1309,.T.);
#875=FACE_OUTER_BOUND('',#1310,.T.);
#876=FACE_OUTER_BOUND('',#1311,.T.);
#877=FACE_OUTER_BOUND('',#1312,.T.);
#878=FACE_OUTER_BOUND('',#1313,.T.);
#879=FACE_OUTER_BOUND('',#1314,.T.);
#880=FACE_OUTER_BOUND('',#1315,.T.);
#881=FACE_OUTER_BOUND('',#1316,.T.);
#882=FACE_OUTER_BOUND('',#1317,.T.);
#883=FACE_OUTER_BOUND('',#1318,.T.);
#884=FACE_OUTER_BOUND('',#1319,.T.);
#885=FACE_OUTER_BOUND('',#1320,.T.);
#886=FACE_OUTER_BOUND('',#1321,.T.);
#887=FACE_OUTER_BOUND('',#1322,.T.);
#888=FACE_OUTER_BOUND('',#1323,.T.);
#889=FACE_OUTER_BOUND('',#1324,.T.);
#890=FACE_OUTER_BOUND('',#1325,.T.);
#891=FACE_OUTER_BOUND('',#1326,.T.);
#892=FACE_OUTER_BOUND('',#1327,.T.);
#893=FACE_OUTER_BOUND('',#1328,.T.);
#894=FACE_OUTER_BOUND('',#1329,.T.);
#895=FACE_OUTER_BOUND('',#1330,.T.);
#896=FACE_OUTER_BOUND('',#1331,.T.);
#897=FACE_OUTER_BOUND('',#1332,.T.);
#898=FACE_OUTER_BOUND('',#1333,.T.);
#899=FACE_OUTER_BOUND('',#1334,.T.);
#900=FACE_OUTER_BOUND('',#1335,.T.);
#901=FACE_OUTER_BOUND('',#1336,.T.);
#902=FACE_OUTER_BOUND('',#1337,.T.);
#903=FACE_OUTER_BOUND('',#1338,.T.);
#904=FACE_OUTER_BOUND('',#1339,.T.);
#905=FACE_OUTER_BOUND('',#1340,.T.);
#906=FACE_OUTER_BOUND('',#1341,.T.);
#907=FACE_OUTER_BOUND('',#1342,.T.);
#908=FACE_OUTER_BOUND('',#1343,.T.);
#909=FACE_OUTER_BOUND('',#1344,.T.);
#910=FACE_OUTER_BOUND('',#1345,.T.);
#911=FACE_OUTER_BOUND('',#1346,.T.);
#912=FACE_OUTER_BOUND('',#1347,.T.);
#913=FACE_OUTER_BOUND('',#1348,.T.);
#914=FACE_OUTER_BOUND('',#1349,.T.);
#915=FACE_OUTER_BOUND('',#1350,.T.);
#916=FACE_OUTER_BOUND('',#1351,.T.);
#917=FACE_OUTER_BOUND('',#1352,.T.);
#918=FACE_OUTER_BOUND('',#1353,.T.);
#919=FACE_OUTER_BOUND('',#1354,.T.);
#920=FACE_OUTER_BOUND('',#1355,.T.);
#921=FACE_OUTER_BOUND('',#1356,.T.);
#922=FACE_OUTER_BOUND('',#1357,.T.);
#923=FACE_OUTER_BOUND('',#1358,.T.);
#924=FACE_OUTER_BOUND('',#1359,.T.);
#925=FACE_OUTER_BOUND('',#1360,.T.);
#926=FACE_OUTER_BOUND('',#1361,.T.);
#927=FACE_OUTER_BOUND('',#1362,.T.);
#928=FACE_OUTER_BOUND('',#1363,.T.);
#929=FACE_OUTER_BOUND('',#1364,.T.);
#930=FACE_OUTER_BOUND('',#1365,.T.);
#931=FACE_OUTER_BOUND('',#1366,.T.);
#932=FACE_OUTER_BOUND('',#1367,.T.);
#933=FACE_OUTER_BOUND('',#1368,.T.);
#934=FACE_OUTER_BOUND('',#1369,.T.);
#935=FACE_OUTER_BOUND('',#1370,.T.);
#936=FACE_OUTER_BOUND('',#1371,.T.);
#937=FACE_OUTER_BOUND('',#1372,.T.);
#938=FACE_OUTER_BOUND('',#1373,.T.);
#939=FACE_OUTER_BOUND('',#1374,.T.);
#940=FACE_OUTER_BOUND('',#1375,.T.);
#941=FACE_OUTER_BOUND('',#1376,.T.);
#942=FACE_OUTER_BOUND('',#1377,.T.);
#943=FACE_OUTER_BOUND('',#1378,.T.);
#944=FACE_OUTER_BOUND('',#1379,.T.);
#945=FACE_OUTER_BOUND('',#1380,.T.);
#946=FACE_OUTER_BOUND('',#1381,.T.);
#947=FACE_OUTER_BOUND('',#1382,.T.);
#948=FACE_OUTER_BOUND('',#1383,.T.);
#949=FACE_OUTER_BOUND('',#1384,.T.);
#950=FACE_OUTER_BOUND('',#1385,.T.);
#951=FACE_OUTER_BOUND('',#1386,.T.);
#952=FACE_OUTER_BOUND('',#1388,.T.);
#953=FACE_OUTER_BOUND('',#1389,.T.);
#954=FACE_OUTER_BOUND('',#1390,.T.);
#955=FACE_OUTER_BOUND('',#1391,.T.);
#956=EDGE_LOOP('',(#4899,#4900,#4901,#4902));
#957=EDGE_LOOP('',(#4903,#4904,#4905,#4906));
#958=EDGE_LOOP('',(#4907,#4908,#4909,#4910));
#959=EDGE_LOOP('',(#4911,#4912,#4913,#4914));
#960=EDGE_LOOP('',(#4915,#4916,#4917,#4918));
#961=EDGE_LOOP('',(#4919,#4920,#4921,#4922));
#962=EDGE_LOOP('',(#4923,#4924,#4925,#4926));
#963=EDGE_LOOP('',(#4927,#4928,#4929,#4930));
#964=EDGE_LOOP('',(#4931,#4932,#4933,#4934));
#965=EDGE_LOOP('',(#4935));
#966=EDGE_LOOP('',(#4936));
#967=EDGE_LOOP('',(#4937));
#968=EDGE_LOOP('',(#4938));
#969=EDGE_LOOP('',(#4939,#4940,#4941,#4942));
#970=EDGE_LOOP('',(#4943));
#971=EDGE_LOOP('',(#4944));
#972=EDGE_LOOP('',(#4945));
#973=EDGE_LOOP('',(#4946));
#974=EDGE_LOOP('',(#4947,#4948,#4949,#4950));
#975=EDGE_LOOP('',(#4951));
#976=EDGE_LOOP('',(#4952));
#977=EDGE_LOOP('',(#4953,#4954,#4955,#4956));
#978=EDGE_LOOP('',(#4957));
#979=EDGE_LOOP('',(#4958));
#980=EDGE_LOOP('',(#4959,#4960));
#981=EDGE_LOOP('',(#4961,#4962,#4963,#4964));
#982=EDGE_LOOP('',(#4965,#4966,#4967,#4968));
#983=EDGE_LOOP('',(#4969,#4970));
#984=EDGE_LOOP('',(#4971,#4972,#4973,#4974,#4975,#4976));
#985=EDGE_LOOP('',(#4977));
#986=EDGE_LOOP('',(#4978,#4979,#4980,#4981,#4982,#4983,#4984,#4985));
#987=EDGE_LOOP('',(#4986));
#988=EDGE_LOOP('',(#4987,#4988,#4989,#4990,#4991,#4992));
#989=EDGE_LOOP('',(#4993));
#990=EDGE_LOOP('',(#4994,#4995,#4996,#4997));
#991=EDGE_LOOP('',(#4998,#4999,#5000,#5001));
#992=EDGE_LOOP('',(#5002,#5003,#5004,#5005));
#993=EDGE_LOOP('',(#5006,#5007,#5008,#5009));
#994=EDGE_LOOP('',(#5010,#5011,#5012,#5013));
#995=EDGE_LOOP('',(#5014,#5015,#5016,#5017,#5018,#5019,#5020,#5021,#5022,
#5023,#5024,#5025));
#996=EDGE_LOOP('',(#5026));
#997=EDGE_LOOP('',(#5027,#5028,#5029,#5030));
#998=EDGE_LOOP('',(#5031,#5032,#5033,#5034));
#999=EDGE_LOOP('',(#5035));
#1000=EDGE_LOOP('',(#5036));
#1001=EDGE_LOOP('',(#5037,#5038,#5039,#5040));
#1002=EDGE_LOOP('',(#5041,#5042,#5043,#5044,#5045,#5046,#5047,#5048));
#1003=EDGE_LOOP('',(#5049));
#1004=EDGE_LOOP('',(#5050,#5051,#5052,#5053));
#1005=EDGE_LOOP('',(#5054,#5055,#5056,#5057));
#1006=EDGE_LOOP('',(#5058));
#1007=EDGE_LOOP('',(#5059,#5060,#5061,#5062));
#1008=EDGE_LOOP('',(#5063,#5064,#5065,#5066));
#1009=EDGE_LOOP('',(#5067));
#1010=EDGE_LOOP('',(#5068,#5069,#5070,#5071));
#1011=EDGE_LOOP('',(#5072,#5073,#5074,#5075,#5076,#5077,#5078,#5079,#5080,
#5081,#5082,#5083));
#1012=EDGE_LOOP('',(#5084));
#1013=EDGE_LOOP('',(#5085,#5086,#5087,#5088));
#1014=EDGE_LOOP('',(#5089,#5090,#5091,#5092));
#1015=EDGE_LOOP('',(#5093,#5094,#5095,#5096));
#1016=EDGE_LOOP('',(#5097,#5098,#5099,#5100));
#1017=EDGE_LOOP('',(#5101,#5102,#5103,#5104));
#1018=EDGE_LOOP('',(#5105,#5106,#5107,#5108));
#1019=EDGE_LOOP('',(#5109,#5110,#5111,#5112,#5113,#5114));
#1020=EDGE_LOOP('',(#5115,#5116,#5117,#5118,#5119,#5120));
#1021=EDGE_LOOP('',(#5121));
#1022=EDGE_LOOP('',(#5122));
#1023=EDGE_LOOP('',(#5123,#5124,#5125,#5126));
#1024=EDGE_LOOP('',(#5127,#5128,#5129,#5130));
#1025=EDGE_LOOP('',(#5131,#5132,#5133,#5134));
#1026=EDGE_LOOP('',(#5135));
#1027=EDGE_LOOP('',(#5136));
#1028=EDGE_LOOP('',(#5137,#5138,#5139,#5140));
#1029=EDGE_LOOP('',(#5141,#5142,#5143,#5144));
#1030=EDGE_LOOP('',(#5145));
#1031=EDGE_LOOP('',(#5146,#5147,#5148,#5149));
#1032=EDGE_LOOP('',(#5150,#5151,#5152,#5153));
#1033=EDGE_LOOP('',(#5154,#5155,#5156,#5157));
#1034=EDGE_LOOP('',(#5158));
#1035=EDGE_LOOP('',(#5159));
#1036=EDGE_LOOP('',(#5160,#5161,#5162,#5163));
#1037=EDGE_LOOP('',(#5164,#5165,#5166,#5167));
#1038=EDGE_LOOP('',(#5168,#5169,#5170,#5171));
#1039=EDGE_LOOP('',(#5172));
#1040=EDGE_LOOP('',(#5173,#5174,#5175,#5176));
#1041=EDGE_LOOP('',(#5177,#5178,#5179,#5180));
#1042=EDGE_LOOP('',(#5181,#5182,#5183,#5184));
#1043=EDGE_LOOP('',(#5185,#5186,#5187,#5188));
#1044=EDGE_LOOP('',(#5189,#5190,#5191,#5192));
#1045=EDGE_LOOP('',(#5193,#5194,#5195,#5196));
#1046=EDGE_LOOP('',(#5197,#5198,#5199,#5200,#5201,#5202));
#1047=EDGE_LOOP('',(#5203,#5204,#5205,#5206,#5207,#5208));
#1048=EDGE_LOOP('',(#5209,#5210,#5211,#5212));
#1049=EDGE_LOOP('',(#5213));
#1050=EDGE_LOOP('',(#5214));
#1051=EDGE_LOOP('',(#5215,#5216,#5217,#5218));
#1052=EDGE_LOOP('',(#5219,#5220,#5221,#5222));
#1053=EDGE_LOOP('',(#5223));
#1054=EDGE_LOOP('',(#5224,#5225,#5226,#5227));
#1055=EDGE_LOOP('',(#5228));
#1056=EDGE_LOOP('',(#5229));
#1057=EDGE_LOOP('',(#5230,#5231,#5232,#5233));
#1058=EDGE_LOOP('',(#5234));
#1059=EDGE_LOOP('',(#5235,#5236,#5237,#5238,#5239));
#1060=EDGE_LOOP('',(#5240,#5241,#5242,#5243));
#1061=EDGE_LOOP('',(#5244,#5245));
#1062=EDGE_LOOP('',(#5246,#5247,#5248,#5249));
#1063=EDGE_LOOP('',(#5250,#5251,#5252,#5253));
#1064=EDGE_LOOP('',(#5254,#5255,#5256,#5257));
#1065=EDGE_LOOP('',(#5258,#5259,#5260,#5261));
#1066=EDGE_LOOP('',(#5262,#5263,#5264,#5265));
#1067=EDGE_LOOP('',(#5266,#5267,#5268,#5269));
#1068=EDGE_LOOP('',(#5270,#5271,#5272,#5273));
#1069=EDGE_LOOP('',(#5274,#5275,#5276,#5277));
#1070=EDGE_LOOP('',(#5278,#5279,#5280,#5281));
#1071=EDGE_LOOP('',(#5282,#5283,#5284,#5285));
#1072=EDGE_LOOP('',(#5286,#5287,#5288,#5289));
#1073=EDGE_LOOP('',(#5290,#5291,#5292,#5293));
#1074=EDGE_LOOP('',(#5294,#5295,#5296,#5297));
#1075=EDGE_LOOP('',(#5298,#5299,#5300,#5301));
#1076=EDGE_LOOP('',(#5302,#5303,#5304,#5305));
#1077=EDGE_LOOP('',(#5306,#5307,#5308,#5309));
#1078=EDGE_LOOP('',(#5310,#5311,#5312,#5313));
#1079=EDGE_LOOP('',(#5314,#5315,#5316,#5317));
#1080=EDGE_LOOP('',(#5318,#5319,#5320,#5321,#5322,#5323,#5324,#5325,#5326,
#5327,#5328,#5329,#5330,#5331,#5332,#5333,#5334,#5335));
#1081=EDGE_LOOP('',(#5336,#5337));
#1082=EDGE_LOOP('',(#5338,#5339));
#1083=EDGE_LOOP('',(#5340,#5341));
#1084=EDGE_LOOP('',(#5342,#5343));
#1085=EDGE_LOOP('',(#5344,#5345));
#1086=EDGE_LOOP('',(#5346,#5347));
#1087=EDGE_LOOP('',(#5348,#5349));
#1088=EDGE_LOOP('',(#5350,#5351));
#1089=EDGE_LOOP('',(#5352,#5353,#5354,#5355,#5356,#5357,#5358,#5359,#5360,
#5361,#5362,#5363,#5364,#5365,#5366,#5367,#5368,#5369,#5370,#5371,#5372,
#5373,#5374,#5375,#5376,#5377,#5378,#5379,#5380,#5381,#5382,#5383,#5384,
#5385));
#1090=EDGE_LOOP('',(#5386));
#1091=EDGE_LOOP('',(#5387,#5388,#5389,#5390));
#1092=EDGE_LOOP('',(#5391,#5392,#5393,#5394));
#1093=EDGE_LOOP('',(#5395,#5396,#5397,#5398));
#1094=EDGE_LOOP('',(#5399,#5400,#5401,#5402));
#1095=EDGE_LOOP('',(#5403,#5404,#5405,#5406));
#1096=EDGE_LOOP('',(#5407,#5408,#5409,#5410));
#1097=EDGE_LOOP('',(#5411,#5412,#5413,#5414));
#1098=EDGE_LOOP('',(#5415,#5416,#5417,#5418));
#1099=EDGE_LOOP('',(#5419,#5420,#5421,#5422));
#1100=EDGE_LOOP('',(#5423,#5424,#5425,#5426));
#1101=EDGE_LOOP('',(#5427,#5428,#5429,#5430));
#1102=EDGE_LOOP('',(#5431,#5432,#5433,#5434));
#1103=EDGE_LOOP('',(#5435,#5436,#5437,#5438));
#1104=EDGE_LOOP('',(#5439,#5440,#5441,#5442));
#1105=EDGE_LOOP('',(#5443,#5444,#5445,#5446));
#1106=EDGE_LOOP('',(#5447,#5448,#5449,#5450));
#1107=EDGE_LOOP('',(#5451,#5452,#5453,#5454));
#1108=EDGE_LOOP('',(#5455,#5456,#5457,#5458));
#1109=EDGE_LOOP('',(#5459,#5460,#5461,#5462,#5463,#5464,#5465,#5466,#5467,
#5468,#5469,#5470,#5471,#5472,#5473,#5474,#5475,#5476));
#1110=EDGE_LOOP('',(#5477,#5478));
#1111=EDGE_LOOP('',(#5479,#5480));
#1112=EDGE_LOOP('',(#5481,#5482));
#1113=EDGE_LOOP('',(#5483,#5484));
#1114=EDGE_LOOP('',(#5485,#5486));
#1115=EDGE_LOOP('',(#5487,#5488));
#1116=EDGE_LOOP('',(#5489,#5490));
#1117=EDGE_LOOP('',(#5491,#5492));
#1118=EDGE_LOOP('',(#5493,#5494,#5495,#5496));
#1119=EDGE_LOOP('',(#5497,#5498,#5499,#5500));
#1120=EDGE_LOOP('',(#5501,#5502,#5503,#5504));
#1121=EDGE_LOOP('',(#5505,#5506,#5507,#5508));
#1122=EDGE_LOOP('',(#5509,#5510,#5511,#5512));
#1123=EDGE_LOOP('',(#5513,#5514,#5515,#5516));
#1124=EDGE_LOOP('',(#5517,#5518,#5519,#5520));
#1125=EDGE_LOOP('',(#5521,#5522,#5523,#5524));
#1126=EDGE_LOOP('',(#5525,#5526,#5527,#5528));
#1127=EDGE_LOOP('',(#5529,#5530,#5531,#5532));
#1128=EDGE_LOOP('',(#5533,#5534,#5535,#5536));
#1129=EDGE_LOOP('',(#5537,#5538,#5539,#5540));
#1130=EDGE_LOOP('',(#5541,#5542,#5543,#5544));
#1131=EDGE_LOOP('',(#5545,#5546,#5547,#5548));
#1132=EDGE_LOOP('',(#5549,#5550,#5551,#5552));
#1133=EDGE_LOOP('',(#5553,#5554,#5555,#5556));
#1134=EDGE_LOOP('',(#5557,#5558,#5559,#5560));
#1135=EDGE_LOOP('',(#5561,#5562,#5563,#5564));
#1136=EDGE_LOOP('',(#5565,#5566,#5567,#5568,#5569,#5570,#5571,#5572,#5573,
#5574,#5575,#5576,#5577,#5578,#5579,#5580,#5581,#5582));
#1137=EDGE_LOOP('',(#5583,#5584));
#1138=EDGE_LOOP('',(#5585,#5586));
#1139=EDGE_LOOP('',(#5587,#5588));
#1140=EDGE_LOOP('',(#5589,#5590));
#1141=EDGE_LOOP('',(#5591,#5592));
#1142=EDGE_LOOP('',(#5593,#5594));
#1143=EDGE_LOOP('',(#5595,#5596));
#1144=EDGE_LOOP('',(#5597,#5598));
#1145=EDGE_LOOP('',(#5599,#5600,#5601,#5602,#5603,#5604,#5605,#5606,#5607,
#5608,#5609,#5610,#5611,#5612,#5613,#5614,#5615,#5616,#5617,#5618,#5619,
#5620,#5621,#5622,#5623,#5624,#5625,#5626,#5627,#5628,#5629));
#1146=EDGE_LOOP('',(#5630));
#1147=EDGE_LOOP('',(#5631));
#1148=EDGE_LOOP('',(#5632));
#1149=EDGE_LOOP('',(#5633,#5634,#5635,#5636,#5637,#5638));
#1150=EDGE_LOOP('',(#5639,#5640,#5641,#5642));
#1151=EDGE_LOOP('',(#5643,#5644));
#1152=EDGE_LOOP('',(#5645,#5646,#5647,#5648));
#1153=EDGE_LOOP('',(#5649,#5650,#5651,#5652));
#1154=EDGE_LOOP('',(#5653,#5654,#5655,#5656));
#1155=EDGE_LOOP('',(#5657,#5658,#5659,#5660));
#1156=EDGE_LOOP('',(#5661,#5662,#5663,#5664));
#1157=EDGE_LOOP('',(#5665,#5666,#5667,#5668));
#1158=EDGE_LOOP('',(#5669,#5670,#5671,#5672));
#1159=EDGE_LOOP('',(#5673,#5674,#5675,#5676));
#1160=EDGE_LOOP('',(#5677,#5678,#5679,#5680));
#1161=EDGE_LOOP('',(#5681,#5682,#5683,#5684));
#1162=EDGE_LOOP('',(#5685,#5686,#5687,#5688));
#1163=EDGE_LOOP('',(#5689,#5690,#5691,#5692));
#1164=EDGE_LOOP('',(#5693,#5694,#5695,#5696));
#1165=EDGE_LOOP('',(#5697,#5698,#5699,#5700));
#1166=EDGE_LOOP('',(#5701,#5702,#5703,#5704));
#1167=EDGE_LOOP('',(#5705,#5706,#5707,#5708));
#1168=EDGE_LOOP('',(#5709,#5710,#5711,#5712));
#1169=EDGE_LOOP('',(#5713,#5714,#5715,#5716));
#1170=EDGE_LOOP('',(#5717,#5718,#5719,#5720,#5721,#5722,#5723,#5724,#5725,
#5726,#5727,#5728,#5729,#5730,#5731,#5732,#5733,#5734));
#1171=EDGE_LOOP('',(#5735,#5736));
#1172=EDGE_LOOP('',(#5737,#5738));
#1173=EDGE_LOOP('',(#5739,#5740));
#1174=EDGE_LOOP('',(#5741,#5742));
#1175=EDGE_LOOP('',(#5743,#5744));
#1176=EDGE_LOOP('',(#5745,#5746));
#1177=EDGE_LOOP('',(#5747,#5748,#5749,#5750,#5751,#5752,#5753,#5754,#5755,
#5756,#5757,#5758,#5759,#5760,#5761,#5762,#5763,#5764,#5765,#5766,#5767,
#5768,#5769,#5770,#5771,#5772,#5773,#5774,#5775,#5776,#5777,#5778,#5779,
#5780));
#1178=EDGE_LOOP('',(#5781));
#1179=EDGE_LOOP('',(#5782,#5783));
#1180=EDGE_LOOP('',(#5784,#5785));
#1181=EDGE_LOOP('',(#5786,#5787,#5788,#5789));
#1182=EDGE_LOOP('',(#5790,#5791,#5792,#5793));
#1183=EDGE_LOOP('',(#5794,#5795,#5796,#5797));
#1184=EDGE_LOOP('',(#5798,#5799,#5800,#5801));
#1185=EDGE_LOOP('',(#5802,#5803,#5804,#5805));
#1186=EDGE_LOOP('',(#5806,#5807,#5808,#5809));
#1187=EDGE_LOOP('',(#5810,#5811,#5812,#5813));
#1188=EDGE_LOOP('',(#5814,#5815,#5816,#5817));
#1189=EDGE_LOOP('',(#5818,#5819,#5820,#5821));
#1190=EDGE_LOOP('',(#5822,#5823,#5824,#5825));
#1191=EDGE_LOOP('',(#5826,#5827,#5828,#5829));
#1192=EDGE_LOOP('',(#5830,#5831,#5832,#5833));
#1193=EDGE_LOOP('',(#5834,#5835,#5836,#5837));
#1194=EDGE_LOOP('',(#5838,#5839,#5840,#5841));
#1195=EDGE_LOOP('',(#5842,#5843,#5844,#5845));
#1196=EDGE_LOOP('',(#5846,#5847,#5848,#5849));
#1197=EDGE_LOOP('',(#5850,#5851,#5852,#5853));
#1198=EDGE_LOOP('',(#5854,#5855,#5856,#5857));
#1199=EDGE_LOOP('',(#5858,#5859,#5860,#5861,#5862,#5863,#5864,#5865,#5866,
#5867,#5868,#5869,#5870,#5871,#5872,#5873,#5874,#5875));
#1200=EDGE_LOOP('',(#5876,#5877));
#1201=EDGE_LOOP('',(#5878,#5879));
#1202=EDGE_LOOP('',(#5880,#5881));
#1203=EDGE_LOOP('',(#5882,#5883));
#1204=EDGE_LOOP('',(#5884,#5885));
#1205=EDGE_LOOP('',(#5886,#5887));
#1206=EDGE_LOOP('',(#5888,#5889));
#1207=EDGE_LOOP('',(#5890,#5891));
#1208=EDGE_LOOP('',(#5892,#5893,#5894,#5895));
#1209=EDGE_LOOP('',(#5896,#5897,#5898,#5899));
#1210=EDGE_LOOP('',(#5900,#5901,#5902,#5903));
#1211=EDGE_LOOP('',(#5904,#5905,#5906,#5907));
#1212=EDGE_LOOP('',(#5908,#5909,#5910,#5911));
#1213=EDGE_LOOP('',(#5912,#5913,#5914,#5915));
#1214=EDGE_LOOP('',(#5916,#5917,#5918,#5919));
#1215=EDGE_LOOP('',(#5920,#5921,#5922,#5923));
#1216=EDGE_LOOP('',(#5924,#5925,#5926,#5927));
#1217=EDGE_LOOP('',(#5928,#5929,#5930,#5931));
#1218=EDGE_LOOP('',(#5932,#5933,#5934,#5935));
#1219=EDGE_LOOP('',(#5936,#5937,#5938,#5939));
#1220=EDGE_LOOP('',(#5940,#5941,#5942,#5943));
#1221=EDGE_LOOP('',(#5944,#5945,#5946,#5947));
#1222=EDGE_LOOP('',(#5948,#5949,#5950,#5951));
#1223=EDGE_LOOP('',(#5952,#5953,#5954,#5955));
#1224=EDGE_LOOP('',(#5956,#5957,#5958,#5959));
#1225=EDGE_LOOP('',(#5960,#5961,#5962,#5963));
#1226=EDGE_LOOP('',(#5964,#5965,#5966,#5967,#5968,#5969,#5970,#5971,#5972,
#5973,#5974,#5975,#5976,#5977,#5978,#5979,#5980,#5981));
#1227=EDGE_LOOP('',(#5982,#5983));
#1228=EDGE_LOOP('',(#5984,#5985));
#1229=EDGE_LOOP('',(#5986,#5987));
#1230=EDGE_LOOP('',(#5988,#5989));
#1231=EDGE_LOOP('',(#5990,#5991));
#1232=EDGE_LOOP('',(#5992,#5993));
#1233=EDGE_LOOP('',(#5994,#5995));
#1234=EDGE_LOOP('',(#5996,#5997));
#1235=EDGE_LOOP('',(#5998,#5999,#6000,#6001,#6002,#6003,#6004,#6005,#6006,
#6007,#6008,#6009,#6010,#6011,#6012,#6013,#6014,#6015,#6016,#6017,#6018,
#6019,#6020,#6021,#6022,#6023,#6024,#6025,#6026,#6027,#6028));
#1236=EDGE_LOOP('',(#6029,#6030));
#1237=EDGE_LOOP('',(#6031));
#1238=EDGE_LOOP('',(#6032));
#1239=EDGE_LOOP('',(#6033,#6034,#6035,#6036,#6037,#6038,#6039,#6040,#6041,
#6042,#6043,#6044,#6045,#6046,#6047,#6048,#6049,#6050,#6051,#6052,#6053,
#6054,#6055,#6056,#6057,#6058,#6059,#6060,#6061,#6062,#6063,#6064,#6065,
#6066,#6067,#6068,#6069,#6070,#6071,#6072,#6073,#6074,#6075,#6076,#6077,
#6078,#6079,#6080,#6081,#6082,#6083,#6084,#6085,#6086));
#1240=EDGE_LOOP('',(#6087,#6088,#6089,#6090));
#1241=EDGE_LOOP('',(#6091,#6092,#6093,#6094));
#1242=EDGE_LOOP('',(#6095,#6096,#6097,#6098));
#1243=EDGE_LOOP('',(#6099,#6100,#6101,#6102));
#1244=EDGE_LOOP('',(#6103,#6104,#6105,#6106));
#1245=EDGE_LOOP('',(#6107,#6108,#6109,#6110));
#1246=EDGE_LOOP('',(#6111,#6112,#6113,#6114,#6115,#6116,#6117,#6118,#6119,
#6120,#6121,#6122,#6123,#6124,#6125,#6126,#6127,#6128,#6129,#6130,#6131,
#6132,#6133,#6134,#6135,#6136,#6137,#6138,#6139,#6140,#6141,#6142,#6143,
#6144,#6145,#6146,#6147,#6148,#6149,#6150,#6151,#6152,#6153,#6154,#6155,
#6156,#6157,#6158,#6159,#6160,#6161,#6162,#6163,#6164));
#1247=EDGE_LOOP('',(#6165,#6166,#6167,#6168,#6169,#6170,#6171,#6172));
#1248=EDGE_LOOP('',(#6173,#6174,#6175,#6176));
#1249=EDGE_LOOP('',(#6177,#6178,#6179,#6180));
#1250=EDGE_LOOP('',(#6181,#6182,#6183,#6184));
#1251=EDGE_LOOP('',(#6185,#6186,#6187,#6188));
#1252=EDGE_LOOP('',(#6189,#6190,#6191,#6192));
#1253=EDGE_LOOP('',(#6193,#6194,#6195,#6196));
#1254=EDGE_LOOP('',(#6197,#6198,#6199,#6200));
#1255=EDGE_LOOP('',(#6201,#6202,#6203,#6204,#6205,#6206,#6207,#6208,#6209,
#6210,#6211,#6212,#6213,#6214));
#1256=EDGE_LOOP('',(#6215,#6216,#6217,#6218));
#1257=EDGE_LOOP('',(#6219,#6220,#6221,#6222));
#1258=EDGE_LOOP('',(#6223,#6224,#6225,#6226));
#1259=EDGE_LOOP('',(#6227,#6228,#6229,#6230));
#1260=EDGE_LOOP('',(#6231,#6232,#6233,#6234));
#1261=EDGE_LOOP('',(#6235,#6236,#6237,#6238));
#1262=EDGE_LOOP('',(#6239,#6240,#6241,#6242));
#1263=EDGE_LOOP('',(#6243,#6244,#6245,#6246));
#1264=EDGE_LOOP('',(#6247,#6248,#6249,#6250));
#1265=EDGE_LOOP('',(#6251,#6252,#6253,#6254));
#1266=EDGE_LOOP('',(#6255,#6256,#6257,#6258));
#1267=EDGE_LOOP('',(#6259,#6260,#6261,#6262,#6263,#6264,#6265,#6266));
#1268=EDGE_LOOP('',(#6267,#6268,#6269,#6270,#6271,#6272,#6273,#6274,#6275,
#6276,#6277,#6278,#6279,#6280));
#1269=EDGE_LOOP('',(#6281,#6282,#6283,#6284,#6285,#6286,#6287,#6288));
#1270=EDGE_LOOP('',(#6289,#6290,#6291,#6292));
#1271=EDGE_LOOP('',(#6293,#6294,#6295,#6296));
#1272=EDGE_LOOP('',(#6297,#6298,#6299,#6300));
#1273=EDGE_LOOP('',(#6301,#6302,#6303,#6304));
#1274=EDGE_LOOP('',(#6305,#6306,#6307,#6308));
#1275=EDGE_LOOP('',(#6309,#6310,#6311,#6312));
#1276=EDGE_LOOP('',(#6313,#6314,#6315,#6316));
#1277=EDGE_LOOP('',(#6317,#6318,#6319,#6320,#6321,#6322,#6323,#6324,#6325,
#6326,#6327,#6328,#6329,#6330));
#1278=EDGE_LOOP('',(#6331,#6332,#6333,#6334));
#1279=EDGE_LOOP('',(#6335,#6336,#6337,#6338));
#1280=EDGE_LOOP('',(#6339,#6340,#6341,#6342));
#1281=EDGE_LOOP('',(#6343,#6344,#6345,#6346));
#1282=EDGE_LOOP('',(#6347,#6348,#6349,#6350));
#1283=EDGE_LOOP('',(#6351,#6352,#6353,#6354));
#1284=EDGE_LOOP('',(#6355,#6356,#6357,#6358));
#1285=EDGE_LOOP('',(#6359,#6360,#6361,#6362));
#1286=EDGE_LOOP('',(#6363,#6364,#6365,#6366));
#1287=EDGE_LOOP('',(#6367,#6368,#6369,#6370));
#1288=EDGE_LOOP('',(#6371,#6372,#6373,#6374));
#1289=EDGE_LOOP('',(#6375,#6376,#6377,#6378,#6379,#6380,#6381,#6382));
#1290=EDGE_LOOP('',(#6383,#6384,#6385,#6386,#6387,#6388,#6389,#6390,#6391,
#6392,#6393,#6394,#6395,#6396));
#1291=EDGE_LOOP('',(#6397,#6398,#6399,#6400,#6401,#6402,#6403,#6404));
#1292=EDGE_LOOP('',(#6405,#6406,#6407,#6408));
#1293=EDGE_LOOP('',(#6409,#6410,#6411,#6412));
#1294=EDGE_LOOP('',(#6413,#6414,#6415,#6416));
#1295=EDGE_LOOP('',(#6417,#6418,#6419,#6420));
#1296=EDGE_LOOP('',(#6421,#6422,#6423,#6424));
#1297=EDGE_LOOP('',(#6425,#6426,#6427,#6428));
#1298=EDGE_LOOP('',(#6429,#6430,#6431,#6432));
#1299=EDGE_LOOP('',(#6433,#6434,#6435,#6436,#6437,#6438,#6439,#6440,#6441,
#6442,#6443,#6444,#6445,#6446));
#1300=EDGE_LOOP('',(#6447,#6448,#6449,#6450));
#1301=EDGE_LOOP('',(#6451,#6452,#6453,#6454));
#1302=EDGE_LOOP('',(#6455,#6456,#6457,#6458));
#1303=EDGE_LOOP('',(#6459,#6460,#6461,#6462));
#1304=EDGE_LOOP('',(#6463,#6464,#6465,#6466));
#1305=EDGE_LOOP('',(#6467,#6468,#6469,#6470));
#1306=EDGE_LOOP('',(#6471,#6472,#6473,#6474));
#1307=EDGE_LOOP('',(#6475,#6476,#6477,#6478));
#1308=EDGE_LOOP('',(#6479,#6480,#6481,#6482));
#1309=EDGE_LOOP('',(#6483,#6484,#6485,#6486));
#1310=EDGE_LOOP('',(#6487,#6488,#6489,#6490));
#1311=EDGE_LOOP('',(#6491,#6492,#6493,#6494,#6495,#6496,#6497,#6498));
#1312=EDGE_LOOP('',(#6499,#6500,#6501,#6502,#6503,#6504,#6505,#6506,#6507,
#6508,#6509,#6510,#6511,#6512));
#1313=EDGE_LOOP('',(#6513,#6514,#6515,#6516,#6517,#6518,#6519,#6520));
#1314=EDGE_LOOP('',(#6521,#6522,#6523,#6524));
#1315=EDGE_LOOP('',(#6525,#6526,#6527,#6528));
#1316=EDGE_LOOP('',(#6529,#6530,#6531,#6532));
#1317=EDGE_LOOP('',(#6533,#6534,#6535,#6536));
#1318=EDGE_LOOP('',(#6537,#6538,#6539,#6540));
#1319=EDGE_LOOP('',(#6541,#6542,#6543,#6544));
#1320=EDGE_LOOP('',(#6545,#6546,#6547,#6548));
#1321=EDGE_LOOP('',(#6549,#6550,#6551,#6552,#6553,#6554,#6555,#6556,#6557,
#6558,#6559,#6560,#6561,#6562));
#1322=EDGE_LOOP('',(#6563,#6564,#6565,#6566));
#1323=EDGE_LOOP('',(#6567,#6568,#6569,#6570));
#1324=EDGE_LOOP('',(#6571,#6572,#6573,#6574));
#1325=EDGE_LOOP('',(#6575,#6576,#6577,#6578));
#1326=EDGE_LOOP('',(#6579,#6580,#6581,#6582));
#1327=EDGE_LOOP('',(#6583,#6584,#6585,#6586));
#1328=EDGE_LOOP('',(#6587,#6588,#6589,#6590));
#1329=EDGE_LOOP('',(#6591,#6592,#6593,#6594));
#1330=EDGE_LOOP('',(#6595,#6596,#6597,#6598));
#1331=EDGE_LOOP('',(#6599,#6600,#6601,#6602));
#1332=EDGE_LOOP('',(#6603,#6604,#6605,#6606));
#1333=EDGE_LOOP('',(#6607,#6608,#6609,#6610,#6611,#6612,#6613,#6614));
#1334=EDGE_LOOP('',(#6615,#6616,#6617,#6618,#6619,#6620,#6621,#6622,#6623,
#6624,#6625,#6626,#6627,#6628));
#1335=EDGE_LOOP('',(#6629,#6630,#6631,#6632,#6633,#6634,#6635,#6636));
#1336=EDGE_LOOP('',(#6637,#6638,#6639,#6640));
#1337=EDGE_LOOP('',(#6641,#6642,#6643,#6644));
#1338=EDGE_LOOP('',(#6645,#6646,#6647,#6648));
#1339=EDGE_LOOP('',(#6649,#6650,#6651,#6652));
#1340=EDGE_LOOP('',(#6653,#6654,#6655,#6656));
#1341=EDGE_LOOP('',(#6657,#6658,#6659,#6660));
#1342=EDGE_LOOP('',(#6661,#6662,#6663,#6664));
#1343=EDGE_LOOP('',(#6665,#6666,#6667,#6668,#6669,#6670,#6671,#6672,#6673,
#6674,#6675,#6676,#6677,#6678));
#1344=EDGE_LOOP('',(#6679,#6680,#6681,#6682));
#1345=EDGE_LOOP('',(#6683,#6684,#6685,#6686));
#1346=EDGE_LOOP('',(#6687,#6688,#6689,#6690));
#1347=EDGE_LOOP('',(#6691,#6692,#6693,#6694));
#1348=EDGE_LOOP('',(#6695,#6696,#6697,#6698));
#1349=EDGE_LOOP('',(#6699,#6700,#6701,#6702));
#1350=EDGE_LOOP('',(#6703,#6704,#6705,#6706));
#1351=EDGE_LOOP('',(#6707,#6708,#6709,#6710));
#1352=EDGE_LOOP('',(#6711,#6712,#6713,#6714));
#1353=EDGE_LOOP('',(#6715,#6716,#6717,#6718));
#1354=EDGE_LOOP('',(#6719,#6720,#6721,#6722));
#1355=EDGE_LOOP('',(#6723,#6724,#6725,#6726,#6727,#6728,#6729,#6730));
#1356=EDGE_LOOP('',(#6731,#6732,#6733,#6734,#6735,#6736,#6737,#6738,#6739,
#6740,#6741,#6742,#6743,#6744));
#1357=EDGE_LOOP('',(#6745,#6746,#6747,#6748,#6749,#6750,#6751,#6752));
#1358=EDGE_LOOP('',(#6753,#6754,#6755,#6756));
#1359=EDGE_LOOP('',(#6757,#6758,#6759,#6760));
#1360=EDGE_LOOP('',(#6761,#6762,#6763,#6764));
#1361=EDGE_LOOP('',(#6765,#6766,#6767,#6768));
#1362=EDGE_LOOP('',(#6769,#6770,#6771,#6772));
#1363=EDGE_LOOP('',(#6773,#6774,#6775,#6776));
#1364=EDGE_LOOP('',(#6777,#6778,#6779,#6780));
#1365=EDGE_LOOP('',(#6781,#6782,#6783,#6784,#6785,#6786,#6787,#6788,#6789,
#6790,#6791,#6792,#6793,#6794));
#1366=EDGE_LOOP('',(#6795,#6796,#6797,#6798));
#1367=EDGE_LOOP('',(#6799,#6800,#6801,#6802));
#1368=EDGE_LOOP('',(#6803,#6804,#6805,#6806));
#1369=EDGE_LOOP('',(#6807,#6808,#6809,#6810));
#1370=EDGE_LOOP('',(#6811,#6812,#6813,#6814));
#1371=EDGE_LOOP('',(#6815,#6816,#6817,#6818));
#1372=EDGE_LOOP('',(#6819,#6820,#6821,#6822));
#1373=EDGE_LOOP('',(#6823,#6824,#6825,#6826));
#1374=EDGE_LOOP('',(#6827,#6828,#6829,#6830));
#1375=EDGE_LOOP('',(#6831,#6832,#6833,#6834));
#1376=EDGE_LOOP('',(#6835,#6836,#6837,#6838));
#1377=EDGE_LOOP('',(#6839,#6840,#6841,#6842,#6843,#6844,#6845,#6846));
#1378=EDGE_LOOP('',(#6847,#6848,#6849,#6850,#6851,#6852,#6853,#6854,#6855,
#6856,#6857,#6858,#6859,#6860));
#1379=EDGE_LOOP('',(#6861,#6862,#6863,#6864));
#1380=EDGE_LOOP('',(#6865,#6866,#6867,#6868));
#1381=EDGE_LOOP('',(#6869,#6870,#6871,#6872));
#1382=EDGE_LOOP('',(#6873,#6874,#6875,#6876));
#1383=EDGE_LOOP('',(#6877,#6878,#6879,#6880));
#1384=EDGE_LOOP('',(#6881,#6882,#6883,#6884));
#1385=EDGE_LOOP('',(#6885,#6886,#6887,#6888,#6889,#6890));
#1386=EDGE_LOOP('',(#6891));
#1387=EDGE_LOOP('',(#6892,#6893,#6894,#6895,#6896,#6897));
#1388=EDGE_LOOP('',(#6898,#6899,#6900,#6901));
#1389=EDGE_LOOP('',(#6902,#6903,#6904,#6905));
#1390=EDGE_LOOP('',(#6906,#6907,#6908,#6909));
#1391=EDGE_LOOP('',(#6910));
#1392=LINE('',#10046,#2264);
#1393=LINE('',#10052,#2265);
#1394=LINE('',#10058,#2266);
#1395=LINE('',#10064,#2267);
#1396=LINE('',#10069,#2268);
#1397=LINE('',#10071,#2269);
#1398=LINE('',#10073,#2270);
#1399=LINE('',#10074,#2271);
#1400=LINE('',#10077,#2272);
#1401=LINE('',#10079,#2273);
#1402=LINE('',#10080,#2274);
#1403=LINE('',#10083,#2275);
#1404=LINE('',#10085,#2276);
#1405=LINE('',#10086,#2277);
#1406=LINE('',#10088,#2278);
#1407=LINE('',#10089,#2279);
#1408=LINE('',#10097,#2280);
#1409=LINE('',#10106,#2281);
#1410=LINE('',#10114,#2282);
#1411=LINE('',#10118,#2283);
#1412=LINE('',#10121,#2284);
#1413=LINE('',#10125,#2285);
#1414=LINE('',#10129,#2286);
#1415=LINE('',#10132,#2287);
#1416=LINE('',#10135,#2288);
#1417=LINE('',#10137,#2289);
#1418=LINE('',#10139,#2290);
#1419=LINE('',#10141,#2291);
#1420=LINE('',#10142,#2292);
#1421=LINE('',#10147,#2293);
#1422=LINE('',#10149,#2294);
#1423=LINE('',#10150,#2295);
#1424=LINE('',#10156,#2296);
#1425=LINE('',#10158,#2297);
#1426=LINE('',#10159,#2298);
#1427=LINE('',#10161,#2299);
#1428=LINE('',#10162,#2300);
#1429=LINE('',#10169,#2301);
#1430=LINE('',#10173,#2302);
#1431=LINE('',#10178,#2303);
#1432=LINE('',#10182,#2304);
#1433=LINE('',#10187,#2305);
#1434=LINE('',#10191,#2306);
#1435=LINE('',#10193,#2307);
#1436=LINE('',#10194,#2308);
#1437=LINE('',#10196,#2309);
#1438=LINE('',#10198,#2310);
#1439=LINE('',#10200,#2311);
#1440=LINE('',#10202,#2312);
#1441=LINE('',#10204,#2313);
#1442=LINE('',#10205,#2314);
#1443=LINE('',#10208,#2315);
#1444=LINE('',#10209,#2316);
#1445=LINE('',#10212,#2317);
#1446=LINE('',#10213,#2318);
#1447=LINE('',#10215,#2319);
#1448=LINE('',#10218,#2320);
#1449=LINE('',#10219,#2321);
#1450=LINE('',#10222,#2322);
#1451=LINE('',#10223,#2323);
#1452=LINE('',#10226,#2324);
#1453=LINE('',#10227,#2325);
#1454=LINE('',#10230,#2326);
#1455=LINE('',#10231,#2327);
#1456=LINE('',#10234,#2328);
#1457=LINE('',#10235,#2329);
#1458=LINE('',#10237,#2330);
#1459=LINE('',#10243,#2331);
#1460=LINE('',#10245,#2332);
#1461=LINE('',#10247,#2333);
#1462=LINE('',#10248,#2334);
#1463=LINE('',#10251,#2335);
#1464=LINE('',#10253,#2336);
#1465=LINE('',#10254,#2337);
#1466=LINE('',#10257,#2338);
#1467=LINE('',#10259,#2339);
#1468=LINE('',#10260,#2340);
#1469=LINE('',#10263,#2341);
#1470=LINE('',#10265,#2342);
#1471=LINE('',#10266,#2343);
#1472=LINE('',#10269,#2344);
#1473=LINE('',#10271,#2345);
#1474=LINE('',#10272,#2346);
#1475=LINE('',#10274,#2347);
#1476=LINE('',#10275,#2348);
#1477=LINE('',#10287,#2349);
#1478=LINE('',#10291,#2350);
#1479=LINE('',#10295,#2351);
#1480=LINE('',#10302,#2352);
#1481=LINE('',#10304,#2353);
#1482=LINE('',#10312,#2354);
#1483=LINE('',#10316,#2355);
#1484=LINE('',#10320,#2356);
#1485=LINE('',#10327,#2357);
#1486=LINE('',#10331,#2358);
#1487=LINE('',#10335,#2359);
#1488=LINE('',#10340,#2360);
#1489=LINE('',#10342,#2361);
#1490=LINE('',#10344,#2362);
#1491=LINE('',#10345,#2363);
#1492=LINE('',#10348,#2364);
#1493=LINE('',#10350,#2365);
#1494=LINE('',#10351,#2366);
#1495=LINE('',#10354,#2367);
#1496=LINE('',#10356,#2368);
#1497=LINE('',#10357,#2369);
#1498=LINE('',#10360,#2370);
#1499=LINE('',#10362,#2371);
#1500=LINE('',#10363,#2372);
#1501=LINE('',#10366,#2373);
#1502=LINE('',#10368,#2374);
#1503=LINE('',#10369,#2375);
#1504=LINE('',#10371,#2376);
#1505=LINE('',#10372,#2377);
#1506=LINE('',#10413,#2378);
#1507=LINE('',#10456,#2379);
#1508=LINE('',#10460,#2380);
#1509=LINE('',#10464,#2381);
#1510=LINE('',#10469,#2382);
#1511=LINE('',#10512,#2383);
#1512=LINE('',#10551,#2384);
#1513=LINE('',#10556,#2385);
#1514=LINE('',#10558,#2386);
#1515=LINE('',#10560,#2387);
#1516=LINE('',#10561,#2388);
#1517=LINE('',#10564,#2389);
#1518=LINE('',#10566,#2390);
#1519=LINE('',#10567,#2391);
#1520=LINE('',#10570,#2392);
#1521=LINE('',#10572,#2393);
#1522=LINE('',#10573,#2394);
#1523=LINE('',#10576,#2395);
#1524=LINE('',#10578,#2396);
#1525=LINE('',#10579,#2397);
#1526=LINE('',#10582,#2398);
#1527=LINE('',#10584,#2399);
#1528=LINE('',#10585,#2400);
#1529=LINE('',#10588,#2401);
#1530=LINE('',#10590,#2402);
#1531=LINE('',#10591,#2403);
#1532=LINE('',#10594,#2404);
#1533=LINE('',#10596,#2405);
#1534=LINE('',#10597,#2406);
#1535=LINE('',#10600,#2407);
#1536=LINE('',#10602,#2408);
#1537=LINE('',#10603,#2409);
#1538=LINE('',#10606,#2410);
#1539=LINE('',#10608,#2411);
#1540=LINE('',#10609,#2412);
#1541=LINE('',#10612,#2413);
#1542=LINE('',#10614,#2414);
#1543=LINE('',#10615,#2415);
#1544=LINE('',#10618,#2416);
#1545=LINE('',#10620,#2417);
#1546=LINE('',#10621,#2418);
#1547=LINE('',#10624,#2419);
#1548=LINE('',#10626,#2420);
#1549=LINE('',#10627,#2421);
#1550=LINE('',#10630,#2422);
#1551=LINE('',#10632,#2423);
#1552=LINE('',#10633,#2424);
#1553=LINE('',#10636,#2425);
#1554=LINE('',#10638,#2426);
#1555=LINE('',#10639,#2427);
#1556=LINE('',#10642,#2428);
#1557=LINE('',#10644,#2429);
#1558=LINE('',#10645,#2430);
#1559=LINE('',#10648,#2431);
#1560=LINE('',#10650,#2432);
#1561=LINE('',#10651,#2433);
#1562=LINE('',#10654,#2434);
#1563=LINE('',#10656,#2435);
#1564=LINE('',#10657,#2436);
#1565=LINE('',#10659,#2437);
#1566=LINE('',#10660,#2438);
#1567=LINE('',#10682,#2439);
#1568=LINE('',#10684,#2440);
#1569=LINE('',#10686,#2441);
#1570=LINE('',#10688,#2442);
#1571=LINE('',#10690,#2443);
#1572=LINE('',#10692,#2444);
#1573=LINE('',#10694,#2445);
#1574=LINE('',#10696,#2446);
#1575=LINE('',#10698,#2447);
#1576=LINE('',#10700,#2448);
#1577=LINE('',#10704,#2449);
#1578=LINE('',#10706,#2450);
#1579=LINE('',#10708,#2451);
#1580=LINE('',#10710,#2452);
#1581=LINE('',#10712,#2453);
#1582=LINE('',#10714,#2454);
#1583=LINE('',#10716,#2455);
#1584=LINE('',#10718,#2456);
#1585=LINE('',#10720,#2457);
#1586=LINE('',#10722,#2458);
#1587=LINE('',#10729,#2459);
#1588=LINE('',#10730,#2460);
#1589=LINE('',#10732,#2461);
#1590=LINE('',#10733,#2462);
#1591=LINE('',#10736,#2463);
#1592=LINE('',#10738,#2464);
#1593=LINE('',#10739,#2465);
#1594=LINE('',#10742,#2466);
#1595=LINE('',#10744,#2467);
#1596=LINE('',#10745,#2468);
#1597=LINE('',#10748,#2469);
#1598=LINE('',#10750,#2470);
#1599=LINE('',#10751,#2471);
#1600=LINE('',#10754,#2472);
#1601=LINE('',#10756,#2473);
#1602=LINE('',#10757,#2474);
#1603=LINE('',#10760,#2475);
#1604=LINE('',#10762,#2476);
#1605=LINE('',#10763,#2477);
#1606=LINE('',#10766,#2478);
#1607=LINE('',#10768,#2479);
#1608=LINE('',#10769,#2480);
#1609=LINE('',#10772,#2481);
#1610=LINE('',#10773,#2482);
#1611=LINE('',#10774,#2483);
#1612=LINE('',#10777,#2484);
#1613=LINE('',#10778,#2485);
#1614=LINE('',#10781,#2486);
#1615=LINE('',#10782,#2487);
#1616=LINE('',#10785,#2488);
#1617=LINE('',#10786,#2489);
#1618=LINE('',#10789,#2490);
#1619=LINE('',#10790,#2491);
#1620=LINE('',#10793,#2492);
#1621=LINE('',#10794,#2493);
#1622=LINE('',#10797,#2494);
#1623=LINE('',#10798,#2495);
#1624=LINE('',#10801,#2496);
#1625=LINE('',#10802,#2497);
#1626=LINE('',#10805,#2498);
#1627=LINE('',#10806,#2499);
#1628=LINE('',#10809,#2500);
#1629=LINE('',#10810,#2501);
#1630=LINE('',#10812,#2502);
#1631=LINE('',#10833,#2503);
#1632=LINE('',#10834,#2504);
#1633=LINE('',#10836,#2505);
#1634=LINE('',#10837,#2506);
#1635=LINE('',#10840,#2507);
#1636=LINE('',#10842,#2508);
#1637=LINE('',#10843,#2509);
#1638=LINE('',#10846,#2510);
#1639=LINE('',#10848,#2511);
#1640=LINE('',#10849,#2512);
#1641=LINE('',#10852,#2513);
#1642=LINE('',#10854,#2514);
#1643=LINE('',#10855,#2515);
#1644=LINE('',#10858,#2516);
#1645=LINE('',#10860,#2517);
#1646=LINE('',#10861,#2518);
#1647=LINE('',#10864,#2519);
#1648=LINE('',#10866,#2520);
#1649=LINE('',#10867,#2521);
#1650=LINE('',#10870,#2522);
#1651=LINE('',#10872,#2523);
#1652=LINE('',#10873,#2524);
#1653=LINE('',#10876,#2525);
#1654=LINE('',#10877,#2526);
#1655=LINE('',#10878,#2527);
#1656=LINE('',#10881,#2528);
#1657=LINE('',#10882,#2529);
#1658=LINE('',#10885,#2530);
#1659=LINE('',#10886,#2531);
#1660=LINE('',#10889,#2532);
#1661=LINE('',#10890,#2533);
#1662=LINE('',#10893,#2534);
#1663=LINE('',#10894,#2535);
#1664=LINE('',#10897,#2536);
#1665=LINE('',#10898,#2537);
#1666=LINE('',#10901,#2538);
#1667=LINE('',#10902,#2539);
#1668=LINE('',#10905,#2540);
#1669=LINE('',#10906,#2541);
#1670=LINE('',#10909,#2542);
#1671=LINE('',#10910,#2543);
#1672=LINE('',#10913,#2544);
#1673=LINE('',#10914,#2545);
#1674=LINE('',#10916,#2546);
#1675=LINE('',#10937,#2547);
#1676=LINE('',#10980,#2548);
#1677=LINE('',#11022,#2549);
#1678=LINE('',#11027,#2550);
#1679=LINE('',#11029,#2551);
#1680=LINE('',#11031,#2552);
#1681=LINE('',#11032,#2553);
#1682=LINE('',#11035,#2554);
#1683=LINE('',#11037,#2555);
#1684=LINE('',#11038,#2556);
#1685=LINE('',#11041,#2557);
#1686=LINE('',#11043,#2558);
#1687=LINE('',#11044,#2559);
#1688=LINE('',#11047,#2560);
#1689=LINE('',#11049,#2561);
#1690=LINE('',#11050,#2562);
#1691=LINE('',#11053,#2563);
#1692=LINE('',#11055,#2564);
#1693=LINE('',#11056,#2565);
#1694=LINE('',#11059,#2566);
#1695=LINE('',#11061,#2567);
#1696=LINE('',#11062,#2568);
#1697=LINE('',#11065,#2569);
#1698=LINE('',#11067,#2570);
#1699=LINE('',#11068,#2571);
#1700=LINE('',#11071,#2572);
#1701=LINE('',#11073,#2573);
#1702=LINE('',#11074,#2574);
#1703=LINE('',#11077,#2575);
#1704=LINE('',#11079,#2576);
#1705=LINE('',#11080,#2577);
#1706=LINE('',#11083,#2578);
#1707=LINE('',#11085,#2579);
#1708=LINE('',#11086,#2580);
#1709=LINE('',#11089,#2581);
#1710=LINE('',#11091,#2582);
#1711=LINE('',#11092,#2583);
#1712=LINE('',#11095,#2584);
#1713=LINE('',#11097,#2585);
#1714=LINE('',#11098,#2586);
#1715=LINE('',#11101,#2587);
#1716=LINE('',#11103,#2588);
#1717=LINE('',#11104,#2589);
#1718=LINE('',#11107,#2590);
#1719=LINE('',#11109,#2591);
#1720=LINE('',#11110,#2592);
#1721=LINE('',#11113,#2593);
#1722=LINE('',#11115,#2594);
#1723=LINE('',#11116,#2595);
#1724=LINE('',#11119,#2596);
#1725=LINE('',#11121,#2597);
#1726=LINE('',#11122,#2598);
#1727=LINE('',#11125,#2599);
#1728=LINE('',#11127,#2600);
#1729=LINE('',#11128,#2601);
#1730=LINE('',#11130,#2602);
#1731=LINE('',#11131,#2603);
#1732=LINE('',#11151,#2604);
#1733=LINE('',#11153,#2605);
#1734=LINE('',#11155,#2606);
#1735=LINE('',#11157,#2607);
#1736=LINE('',#11159,#2608);
#1737=LINE('',#11161,#2609);
#1738=LINE('',#11163,#2610);
#1739=LINE('',#11165,#2611);
#1740=LINE('',#11167,#2612);
#1741=LINE('',#11169,#2613);
#1742=LINE('',#11173,#2614);
#1743=LINE('',#11175,#2615);
#1744=LINE('',#11177,#2616);
#1745=LINE('',#11179,#2617);
#1746=LINE('',#11181,#2618);
#1747=LINE('',#11183,#2619);
#1748=LINE('',#11185,#2620);
#1749=LINE('',#11187,#2621);
#1750=LINE('',#11189,#2622);
#1751=LINE('',#11191,#2623);
#1752=LINE('',#11200,#2624);
#1753=LINE('',#11201,#2625);
#1754=LINE('',#11202,#2626);
#1755=LINE('',#11205,#2627);
#1756=LINE('',#11206,#2628);
#1757=LINE('',#11209,#2629);
#1758=LINE('',#11210,#2630);
#1759=LINE('',#11213,#2631);
#1760=LINE('',#11214,#2632);
#1761=LINE('',#11217,#2633);
#1762=LINE('',#11218,#2634);
#1763=LINE('',#11221,#2635);
#1764=LINE('',#11222,#2636);
#1765=LINE('',#11225,#2637);
#1766=LINE('',#11226,#2638);
#1767=LINE('',#11229,#2639);
#1768=LINE('',#11230,#2640);
#1769=LINE('',#11233,#2641);
#1770=LINE('',#11234,#2642);
#1771=LINE('',#11237,#2643);
#1772=LINE('',#11239,#2644);
#1773=LINE('',#11240,#2645);
#1774=LINE('',#11243,#2646);
#1775=LINE('',#11245,#2647);
#1776=LINE('',#11246,#2648);
#1777=LINE('',#11249,#2649);
#1778=LINE('',#11251,#2650);
#1779=LINE('',#11252,#2651);
#1780=LINE('',#11255,#2652);
#1781=LINE('',#11257,#2653);
#1782=LINE('',#11258,#2654);
#1783=LINE('',#11261,#2655);
#1784=LINE('',#11263,#2656);
#1785=LINE('',#11264,#2657);
#1786=LINE('',#11267,#2658);
#1787=LINE('',#11269,#2659);
#1788=LINE('',#11270,#2660);
#1789=LINE('',#11273,#2661);
#1790=LINE('',#11275,#2662);
#1791=LINE('',#11276,#2663);
#1792=LINE('',#11279,#2664);
#1793=LINE('',#11280,#2665);
#1794=LINE('',#11281,#2666);
#1795=LINE('',#11283,#2667);
#1796=LINE('',#11304,#2668);
#1797=LINE('',#11305,#2669);
#1798=LINE('',#11306,#2670);
#1799=LINE('',#11309,#2671);
#1800=LINE('',#11310,#2672);
#1801=LINE('',#11313,#2673);
#1802=LINE('',#11314,#2674);
#1803=LINE('',#11317,#2675);
#1804=LINE('',#11318,#2676);
#1805=LINE('',#11321,#2677);
#1806=LINE('',#11322,#2678);
#1807=LINE('',#11325,#2679);
#1808=LINE('',#11326,#2680);
#1809=LINE('',#11329,#2681);
#1810=LINE('',#11330,#2682);
#1811=LINE('',#11333,#2683);
#1812=LINE('',#11334,#2684);
#1813=LINE('',#11337,#2685);
#1814=LINE('',#11338,#2686);
#1815=LINE('',#11341,#2687);
#1816=LINE('',#11343,#2688);
#1817=LINE('',#11344,#2689);
#1818=LINE('',#11347,#2690);
#1819=LINE('',#11349,#2691);
#1820=LINE('',#11350,#2692);
#1821=LINE('',#11353,#2693);
#1822=LINE('',#11355,#2694);
#1823=LINE('',#11356,#2695);
#1824=LINE('',#11359,#2696);
#1825=LINE('',#11361,#2697);
#1826=LINE('',#11362,#2698);
#1827=LINE('',#11365,#2699);
#1828=LINE('',#11367,#2700);
#1829=LINE('',#11368,#2701);
#1830=LINE('',#11371,#2702);
#1831=LINE('',#11373,#2703);
#1832=LINE('',#11374,#2704);
#1833=LINE('',#11377,#2705);
#1834=LINE('',#11379,#2706);
#1835=LINE('',#11380,#2707);
#1836=LINE('',#11383,#2708);
#1837=LINE('',#11384,#2709);
#1838=LINE('',#11385,#2710);
#1839=LINE('',#11387,#2711);
#1840=LINE('',#11408,#2712);
#1841=LINE('',#11414,#2713);
#1842=LINE('',#11416,#2714);
#1843=LINE('',#11418,#2715);
#1844=LINE('',#11420,#2716);
#1845=LINE('',#11422,#2717);
#1846=LINE('',#11424,#2718);
#1847=LINE('',#11426,#2719);
#1848=LINE('',#11428,#2720);
#1849=LINE('',#11432,#2721);
#1850=LINE('',#11434,#2722);
#1851=LINE('',#11436,#2723);
#1852=LINE('',#11438,#2724);
#1853=LINE('',#11440,#2725);
#1854=LINE('',#11442,#2726);
#1855=LINE('',#11444,#2727);
#1856=LINE('',#11446,#2728);
#1857=LINE('',#11450,#2729);
#1858=LINE('',#11452,#2730);
#1859=LINE('',#11454,#2731);
#1860=LINE('',#11456,#2732);
#1861=LINE('',#11458,#2733);
#1862=LINE('',#11460,#2734);
#1863=LINE('',#11462,#2735);
#1864=LINE('',#11464,#2736);
#1865=LINE('',#11468,#2737);
#1866=LINE('',#11470,#2738);
#1867=LINE('',#11472,#2739);
#1868=LINE('',#11474,#2740);
#1869=LINE('',#11476,#2741);
#1870=LINE('',#11478,#2742);
#1871=LINE('',#11480,#2743);
#1872=LINE('',#11482,#2744);
#1873=LINE('',#11486,#2745);
#1874=LINE('',#11488,#2746);
#1875=LINE('',#11490,#2747);
#1876=LINE('',#11492,#2748);
#1877=LINE('',#11494,#2749);
#1878=LINE('',#11496,#2750);
#1879=LINE('',#11498,#2751);
#1880=LINE('',#11500,#2752);
#1881=LINE('',#11504,#2753);
#1882=LINE('',#11506,#2754);
#1883=LINE('',#11508,#2755);
#1884=LINE('',#11510,#2756);
#1885=LINE('',#11512,#2757);
#1886=LINE('',#11514,#2758);
#1887=LINE('',#11516,#2759);
#1888=LINE('',#11518,#2760);
#1889=LINE('',#11522,#2761);
#1890=LINE('',#11525,#2762);
#1891=LINE('',#11528,#2763);
#1892=LINE('',#11531,#2764);
#1893=LINE('',#11534,#2765);
#1894=LINE('',#11537,#2766);
#1895=LINE('',#11540,#2767);
#1896=LINE('',#11542,#2768);
#1897=LINE('',#11546,#2769);
#1898=LINE('',#11548,#2770);
#1899=LINE('',#11552,#2771);
#1900=LINE('',#11554,#2772);
#1901=LINE('',#11558,#2773);
#1902=LINE('',#11560,#2774);
#1903=LINE('',#11562,#2775);
#1904=LINE('',#11564,#2776);
#1905=LINE('',#11566,#2777);
#1906=LINE('',#11568,#2778);
#1907=LINE('',#11570,#2779);
#1908=LINE('',#11572,#2780);
#1909=LINE('',#11573,#2781);
#1910=LINE('',#11575,#2782);
#1911=LINE('',#11577,#2783);
#1912=LINE('',#11579,#2784);
#1913=LINE('',#11581,#2785);
#1914=LINE('',#11583,#2786);
#1915=LINE('',#11585,#2787);
#1916=LINE('',#11587,#2788);
#1917=LINE('',#11588,#2789);
#1918=LINE('',#11590,#2790);
#1919=LINE('',#11592,#2791);
#1920=LINE('',#11594,#2792);
#1921=LINE('',#11596,#2793);
#1922=LINE('',#11598,#2794);
#1923=LINE('',#11600,#2795);
#1924=LINE('',#11602,#2796);
#1925=LINE('',#11603,#2797);
#1926=LINE('',#11605,#2798);
#1927=LINE('',#11607,#2799);
#1928=LINE('',#11609,#2800);
#1929=LINE('',#11611,#2801);
#1930=LINE('',#11613,#2802);
#1931=LINE('',#11615,#2803);
#1932=LINE('',#11617,#2804);
#1933=LINE('',#11618,#2805);
#1934=LINE('',#11620,#2806);
#1935=LINE('',#11622,#2807);
#1936=LINE('',#11624,#2808);
#1937=LINE('',#11626,#2809);
#1938=LINE('',#11628,#2810);
#1939=LINE('',#11630,#2811);
#1940=LINE('',#11632,#2812);
#1941=LINE('',#11633,#2813);
#1942=LINE('',#11635,#2814);
#1943=LINE('',#11637,#2815);
#1944=LINE('',#11639,#2816);
#1945=LINE('',#11641,#2817);
#1946=LINE('',#11643,#2818);
#1947=LINE('',#11645,#2819);
#1948=LINE('',#11646,#2820);
#1949=LINE('',#11649,#2821);
#1950=LINE('',#11651,#2822);
#1951=LINE('',#11653,#2823);
#1952=LINE('',#11655,#2824);
#1953=LINE('',#11656,#2825);
#1954=LINE('',#11659,#2826);
#1955=LINE('',#11660,#2827);
#1956=LINE('',#11663,#2828);
#1957=LINE('',#11664,#2829);
#1958=LINE('',#11667,#2830);
#1959=LINE('',#11668,#2831);
#1960=LINE('',#11671,#2832);
#1961=LINE('',#11672,#2833);
#1962=LINE('',#11675,#2834);
#1963=LINE('',#11676,#2835);
#1964=LINE('',#11679,#2836);
#1965=LINE('',#11680,#2837);
#1966=LINE('',#11683,#2838);
#1967=LINE('',#11684,#2839);
#1968=LINE('',#11688,#2840);
#1969=LINE('',#11690,#2841);
#1970=LINE('',#11692,#2842);
#1971=LINE('',#11694,#2843);
#1972=LINE('',#11696,#2844);
#1973=LINE('',#11697,#2845);
#1974=LINE('',#11699,#2846);
#1975=LINE('',#11701,#2847);
#1976=LINE('',#11703,#2848);
#1977=LINE('',#11705,#2849);
#1978=LINE('',#11707,#2850);
#1979=LINE('',#11708,#2851);
#1980=LINE('',#11710,#2852);
#1981=LINE('',#11711,#2853);
#1982=LINE('',#11713,#2854);
#1983=LINE('',#11715,#2855);
#1984=LINE('',#11717,#2856);
#1985=LINE('',#11721,#2857);
#1986=LINE('',#11722,#2858);
#1987=LINE('',#11725,#2859);
#1988=LINE('',#11726,#2860);
#1989=LINE('',#11729,#2861);
#1990=LINE('',#11730,#2862);
#1991=LINE('',#11733,#2863);
#1992=LINE('',#11734,#2864);
#1993=LINE('',#11737,#2865);
#1994=LINE('',#11738,#2866);
#1995=LINE('',#11741,#2867);
#1996=LINE('',#11742,#2868);
#1997=LINE('',#11744,#2869);
#1998=LINE('',#11748,#2870);
#1999=LINE('',#11750,#2871);
#2000=LINE('',#11752,#2872);
#2001=LINE('',#11754,#2873);
#2002=LINE('',#11755,#2874);
#2003=LINE('',#11758,#2875);
#2004=LINE('',#11759,#2876);
#2005=LINE('',#11762,#2877);
#2006=LINE('',#11763,#2878);
#2007=LINE('',#11766,#2879);
#2008=LINE('',#11767,#2880);
#2009=LINE('',#11770,#2881);
#2010=LINE('',#11771,#2882);
#2011=LINE('',#11774,#2883);
#2012=LINE('',#11775,#2884);
#2013=LINE('',#11778,#2885);
#2014=LINE('',#11779,#2886);
#2015=LINE('',#11782,#2887);
#2016=LINE('',#11783,#2888);
#2017=LINE('',#11787,#2889);
#2018=LINE('',#11789,#2890);
#2019=LINE('',#11791,#2891);
#2020=LINE('',#11793,#2892);
#2021=LINE('',#11795,#2893);
#2022=LINE('',#11796,#2894);
#2023=LINE('',#11798,#2895);
#2024=LINE('',#11800,#2896);
#2025=LINE('',#11802,#2897);
#2026=LINE('',#11804,#2898);
#2027=LINE('',#11806,#2899);
#2028=LINE('',#11807,#2900);
#2029=LINE('',#11809,#2901);
#2030=LINE('',#11810,#2902);
#2031=LINE('',#11812,#2903);
#2032=LINE('',#11814,#2904);
#2033=LINE('',#11816,#2905);
#2034=LINE('',#11820,#2906);
#2035=LINE('',#11821,#2907);
#2036=LINE('',#11824,#2908);
#2037=LINE('',#11825,#2909);
#2038=LINE('',#11828,#2910);
#2039=LINE('',#11829,#2911);
#2040=LINE('',#11832,#2912);
#2041=LINE('',#11833,#2913);
#2042=LINE('',#11836,#2914);
#2043=LINE('',#11837,#2915);
#2044=LINE('',#11840,#2916);
#2045=LINE('',#11841,#2917);
#2046=LINE('',#11843,#2918);
#2047=LINE('',#11847,#2919);
#2048=LINE('',#11849,#2920);
#2049=LINE('',#11851,#2921);
#2050=LINE('',#11853,#2922);
#2051=LINE('',#11854,#2923);
#2052=LINE('',#11857,#2924);
#2053=LINE('',#11858,#2925);
#2054=LINE('',#11861,#2926);
#2055=LINE('',#11862,#2927);
#2056=LINE('',#11865,#2928);
#2057=LINE('',#11866,#2929);
#2058=LINE('',#11869,#2930);
#2059=LINE('',#11870,#2931);
#2060=LINE('',#11873,#2932);
#2061=LINE('',#11874,#2933);
#2062=LINE('',#11877,#2934);
#2063=LINE('',#11878,#2935);
#2064=LINE('',#11881,#2936);
#2065=LINE('',#11882,#2937);
#2066=LINE('',#11886,#2938);
#2067=LINE('',#11888,#2939);
#2068=LINE('',#11890,#2940);
#2069=LINE('',#11892,#2941);
#2070=LINE('',#11894,#2942);
#2071=LINE('',#11895,#2943);
#2072=LINE('',#11897,#2944);
#2073=LINE('',#11899,#2945);
#2074=LINE('',#11901,#2946);
#2075=LINE('',#11903,#2947);
#2076=LINE('',#11905,#2948);
#2077=LINE('',#11906,#2949);
#2078=LINE('',#11908,#2950);
#2079=LINE('',#11909,#2951);
#2080=LINE('',#11911,#2952);
#2081=LINE('',#11913,#2953);
#2082=LINE('',#11915,#2954);
#2083=LINE('',#11919,#2955);
#2084=LINE('',#11920,#2956);
#2085=LINE('',#11923,#2957);
#2086=LINE('',#11924,#2958);
#2087=LINE('',#11927,#2959);
#2088=LINE('',#11928,#2960);
#2089=LINE('',#11931,#2961);
#2090=LINE('',#11932,#2962);
#2091=LINE('',#11935,#2963);
#2092=LINE('',#11936,#2964);
#2093=LINE('',#11939,#2965);
#2094=LINE('',#11940,#2966);
#2095=LINE('',#11942,#2967);
#2096=LINE('',#11946,#2968);
#2097=LINE('',#11948,#2969);
#2098=LINE('',#11950,#2970);
#2099=LINE('',#11952,#2971);
#2100=LINE('',#11953,#2972);
#2101=LINE('',#11956,#2973);
#2102=LINE('',#11957,#2974);
#2103=LINE('',#11960,#2975);
#2104=LINE('',#11961,#2976);
#2105=LINE('',#11964,#2977);
#2106=LINE('',#11965,#2978);
#2107=LINE('',#11968,#2979);
#2108=LINE('',#11969,#2980);
#2109=LINE('',#11972,#2981);
#2110=LINE('',#11973,#2982);
#2111=LINE('',#11976,#2983);
#2112=LINE('',#11977,#2984);
#2113=LINE('',#11980,#2985);
#2114=LINE('',#11981,#2986);
#2115=LINE('',#11985,#2987);
#2116=LINE('',#11987,#2988);
#2117=LINE('',#11989,#2989);
#2118=LINE('',#11991,#2990);
#2119=LINE('',#11993,#2991);
#2120=LINE('',#11994,#2992);
#2121=LINE('',#11996,#2993);
#2122=LINE('',#11998,#2994);
#2123=LINE('',#12000,#2995);
#2124=LINE('',#12002,#2996);
#2125=LINE('',#12004,#2997);
#2126=LINE('',#12005,#2998);
#2127=LINE('',#12007,#2999);
#2128=LINE('',#12008,#3000);
#2129=LINE('',#12010,#3001);
#2130=LINE('',#12012,#3002);
#2131=LINE('',#12014,#3003);
#2132=LINE('',#12018,#3004);
#2133=LINE('',#12019,#3005);
#2134=LINE('',#12022,#3006);
#2135=LINE('',#12023,#3007);
#2136=LINE('',#12026,#3008);
#2137=LINE('',#12027,#3009);
#2138=LINE('',#12030,#3010);
#2139=LINE('',#12031,#3011);
#2140=LINE('',#12034,#3012);
#2141=LINE('',#12035,#3013);
#2142=LINE('',#12038,#3014);
#2143=LINE('',#12039,#3015);
#2144=LINE('',#12041,#3016);
#2145=LINE('',#12045,#3017);
#2146=LINE('',#12047,#3018);
#2147=LINE('',#12049,#3019);
#2148=LINE('',#12051,#3020);
#2149=LINE('',#12052,#3021);
#2150=LINE('',#12055,#3022);
#2151=LINE('',#12056,#3023);
#2152=LINE('',#12059,#3024);
#2153=LINE('',#12060,#3025);
#2154=LINE('',#12063,#3026);
#2155=LINE('',#12064,#3027);
#2156=LINE('',#12067,#3028);
#2157=LINE('',#12068,#3029);
#2158=LINE('',#12071,#3030);
#2159=LINE('',#12072,#3031);
#2160=LINE('',#12075,#3032);
#2161=LINE('',#12076,#3033);
#2162=LINE('',#12079,#3034);
#2163=LINE('',#12080,#3035);
#2164=LINE('',#12084,#3036);
#2165=LINE('',#12086,#3037);
#2166=LINE('',#12088,#3038);
#2167=LINE('',#12090,#3039);
#2168=LINE('',#12092,#3040);
#2169=LINE('',#12093,#3041);
#2170=LINE('',#12095,#3042);
#2171=LINE('',#12097,#3043);
#2172=LINE('',#12099,#3044);
#2173=LINE('',#12101,#3045);
#2174=LINE('',#12103,#3046);
#2175=LINE('',#12104,#3047);
#2176=LINE('',#12106,#3048);
#2177=LINE('',#12107,#3049);
#2178=LINE('',#12109,#3050);
#2179=LINE('',#12111,#3051);
#2180=LINE('',#12113,#3052);
#2181=LINE('',#12117,#3053);
#2182=LINE('',#12118,#3054);
#2183=LINE('',#12121,#3055);
#2184=LINE('',#12122,#3056);
#2185=LINE('',#12125,#3057);
#2186=LINE('',#12126,#3058);
#2187=LINE('',#12129,#3059);
#2188=LINE('',#12130,#3060);
#2189=LINE('',#12133,#3061);
#2190=LINE('',#12134,#3062);
#2191=LINE('',#12137,#3063);
#2192=LINE('',#12138,#3064);
#2193=LINE('',#12140,#3065);
#2194=LINE('',#12144,#3066);
#2195=LINE('',#12146,#3067);
#2196=LINE('',#12148,#3068);
#2197=LINE('',#12150,#3069);
#2198=LINE('',#12151,#3070);
#2199=LINE('',#12154,#3071);
#2200=LINE('',#12155,#3072);
#2201=LINE('',#12158,#3073);
#2202=LINE('',#12159,#3074);
#2203=LINE('',#12162,#3075);
#2204=LINE('',#12163,#3076);
#2205=LINE('',#12166,#3077);
#2206=LINE('',#12167,#3078);
#2207=LINE('',#12170,#3079);
#2208=LINE('',#12171,#3080);
#2209=LINE('',#12174,#3081);
#2210=LINE('',#12175,#3082);
#2211=LINE('',#12178,#3083);
#2212=LINE('',#12179,#3084);
#2213=LINE('',#12183,#3085);
#2214=LINE('',#12185,#3086);
#2215=LINE('',#12187,#3087);
#2216=LINE('',#12189,#3088);
#2217=LINE('',#12191,#3089);
#2218=LINE('',#12192,#3090);
#2219=LINE('',#12194,#3091);
#2220=LINE('',#12196,#3092);
#2221=LINE('',#12198,#3093);
#2222=LINE('',#12200,#3094);
#2223=LINE('',#12202,#3095);
#2224=LINE('',#12203,#3096);
#2225=LINE('',#12205,#3097);
#2226=LINE('',#12206,#3098);
#2227=LINE('',#12208,#3099);
#2228=LINE('',#12210,#3100);
#2229=LINE('',#12212,#3101);
#2230=LINE('',#12216,#3102);
#2231=LINE('',#12217,#3103);
#2232=LINE('',#12220,#3104);
#2233=LINE('',#12221,#3105);
#2234=LINE('',#12224,#3106);
#2235=LINE('',#12225,#3107);
#2236=LINE('',#12228,#3108);
#2237=LINE('',#12229,#3109);
#2238=LINE('',#12232,#3110);
#2239=LINE('',#12233,#3111);
#2240=LINE('',#12236,#3112);
#2241=LINE('',#12237,#3113);
#2242=LINE('',#12239,#3114);
#2243=LINE('',#12248,#3115);
#2244=LINE('',#12250,#3116);
#2245=LINE('',#12252,#3117);
#2246=LINE('',#12253,#3118);
#2247=LINE('',#12256,#3119);
#2248=LINE('',#12258,#3120);
#2249=LINE('',#12259,#3121);
#2250=LINE('',#12262,#3122);
#2251=LINE('',#12264,#3123);
#2252=LINE('',#12265,#3124);
#2253=LINE('',#12268,#3125);
#2254=LINE('',#12270,#3126);
#2255=LINE('',#12271,#3127);
#2256=LINE('',#12274,#3128);
#2257=LINE('',#12276,#3129);
#2258=LINE('',#12277,#3130);
#2259=LINE('',#12279,#3131);
#2260=LINE('',#12280,#3132);
#2261=LINE('',#12288,#3133);
#2262=LINE('',#12292,#3134);
#2263=LINE('',#12296,#3135);
#2264=VECTOR('',#8052,0.21);
#2265=VECTOR('',#8059,0.21);
#2266=VECTOR('',#8066,0.21);
#2267=VECTOR('',#8073,0.21);
#2268=VECTOR('',#8078,1.);
#2269=VECTOR('',#8079,1.);
#2270=VECTOR('',#8080,1.);
#2271=VECTOR('',#8081,1.);
#2272=VECTOR('',#8084,1.);
#2273=VECTOR('',#8085,1.);
#2274=VECTOR('',#8086,1.);
#2275=VECTOR('',#8089,1.);
#2276=VECTOR('',#8090,1.);
#2277=VECTOR('',#8091,1.);
#2278=VECTOR('',#8094,1.);
#2279=VECTOR('',#8095,1.);
#2280=VECTOR('',#8106,0.6);
#2281=VECTOR('',#8119,0.6);
#2282=VECTOR('',#8130,1.);
#2283=VECTOR('',#8135,1.);
#2284=VECTOR('',#8138,1.);
#2285=VECTOR('',#8141,1.);
#2286=VECTOR('',#8144,1.);
#2287=VECTOR('',#8149,1.);
#2288=VECTOR('',#8152,1.);
#2289=VECTOR('',#8153,1.);
#2290=VECTOR('',#8154,1.);
#2291=VECTOR('',#8155,1.);
#2292=VECTOR('',#8156,1.);
#2293=VECTOR('',#8161,1.);
#2294=VECTOR('',#8162,1.);
#2295=VECTOR('',#8163,1.);
#2296=VECTOR('',#8168,1.);
#2297=VECTOR('',#8169,1.);
#2298=VECTOR('',#8170,1.);
#2299=VECTOR('',#8171,1.);
#2300=VECTOR('',#8172,1.);
#2301=VECTOR('',#8179,0.225);
#2302=VECTOR('',#8184,0.165);
#2303=VECTOR('',#8191,0.275);
#2304=VECTOR('',#8196,0.275);
#2305=VECTOR('',#8201,0.6);
#2306=VECTOR('',#8206,1.);
#2307=VECTOR('',#8207,1.);
#2308=VECTOR('',#8208,1.);
#2309=VECTOR('',#8209,1.);
#2310=VECTOR('',#8210,1.);
#2311=VECTOR('',#8211,1.);
#2312=VECTOR('',#8212,1.);
#2313=VECTOR('',#8213,1.);
#2314=VECTOR('',#8214,1.);
#2315=VECTOR('',#8217,1.);
#2316=VECTOR('',#8218,1.);
#2317=VECTOR('',#8221,1.);
#2318=VECTOR('',#8222,1.);
#2319=VECTOR('',#8225,1.);
#2320=VECTOR('',#8228,1.);
#2321=VECTOR('',#8229,1.);
#2322=VECTOR('',#8232,1.);
#2323=VECTOR('',#8233,1.);
#2324=VECTOR('',#8236,1.);
#2325=VECTOR('',#8237,1.);
#2326=VECTOR('',#8240,1.);
#2327=VECTOR('',#8241,1.);
#2328=VECTOR('',#8244,1.);
#2329=VECTOR('',#8245,1.);
#2330=VECTOR('',#8248,1.);
#2331=VECTOR('',#8255,1.);
#2332=VECTOR('',#8256,1.);
#2333=VECTOR('',#8257,1.);
#2334=VECTOR('',#8258,1.);
#2335=VECTOR('',#8261,1.);
#2336=VECTOR('',#8262,1.);
#2337=VECTOR('',#8263,1.);
#2338=VECTOR('',#8266,1.);
#2339=VECTOR('',#8267,1.);
#2340=VECTOR('',#8268,1.);
#2341=VECTOR('',#8271,1.);
#2342=VECTOR('',#8272,1.);
#2343=VECTOR('',#8273,1.);
#2344=VECTOR('',#8276,1.);
#2345=VECTOR('',#8277,1.);
#2346=VECTOR('',#8278,1.);
#2347=VECTOR('',#8281,1.);
#2348=VECTOR('',#8282,1.);
#2349=VECTOR('',#8299,0.4);
#2350=VECTOR('',#8304,0.425);
#2351=VECTOR('',#8309,0.41);
#2352=VECTOR('',#8318,0.26);
#2353=VECTOR('',#8321,0.25);
#2354=VECTOR('',#8332,0.325);
#2355=VECTOR('',#8337,0.35);
#2356=VECTOR('',#8342,0.335);
#2357=VECTOR('',#8351,0.21);
#2358=VECTOR('',#8356,0.2);
#2359=VECTOR('',#8361,0.18);
#2360=VECTOR('',#8366,1.);
#2361=VECTOR('',#8367,1.);
#2362=VECTOR('',#8368,1.);
#2363=VECTOR('',#8369,1.);
#2364=VECTOR('',#8372,1.);
#2365=VECTOR('',#8373,1.);
#2366=VECTOR('',#8374,1.);
#2367=VECTOR('',#8377,1.);
#2368=VECTOR('',#8378,1.);
#2369=VECTOR('',#8379,1.);
#2370=VECTOR('',#8382,1.);
#2371=VECTOR('',#8383,1.);
#2372=VECTOR('',#8384,1.);
#2373=VECTOR('',#8387,1.);
#2374=VECTOR('',#8388,1.);
#2375=VECTOR('',#8389,1.);
#2376=VECTOR('',#8392,1.);
#2377=VECTOR('',#8393,1.);
#2378=VECTOR('',#8402,0.21);
#2379=VECTOR('',#8413,1.075);
#2380=VECTOR('',#8418,1.1);
#2381=VECTOR('',#8423,1.075);
#2382=VECTOR('',#8430,0.6);
#2383=VECTOR('',#8437,0.21);
#2384=VECTOR('',#8442,0.6);
#2385=VECTOR('',#8447,1.);
#2386=VECTOR('',#8448,1.);
#2387=VECTOR('',#8449,1.);
#2388=VECTOR('',#8450,1.);
#2389=VECTOR('',#8453,1.);
#2390=VECTOR('',#8454,1.);
#2391=VECTOR('',#8455,1.);
#2392=VECTOR('',#8458,1.);
#2393=VECTOR('',#8459,1.);
#2394=VECTOR('',#8460,1.);
#2395=VECTOR('',#8463,1.);
#2396=VECTOR('',#8464,1.);
#2397=VECTOR('',#8465,1.);
#2398=VECTOR('',#8468,1.);
#2399=VECTOR('',#8469,1.);
#2400=VECTOR('',#8470,1.);
#2401=VECTOR('',#8473,1.);
#2402=VECTOR('',#8474,1.);
#2403=VECTOR('',#8475,1.);
#2404=VECTOR('',#8478,1.);
#2405=VECTOR('',#8479,1.);
#2406=VECTOR('',#8480,1.);
#2407=VECTOR('',#8483,1.);
#2408=VECTOR('',#8484,1.);
#2409=VECTOR('',#8485,1.);
#2410=VECTOR('',#8488,1.);
#2411=VECTOR('',#8489,1.);
#2412=VECTOR('',#8490,1.);
#2413=VECTOR('',#8493,1.);
#2414=VECTOR('',#8494,1.);
#2415=VECTOR('',#8495,1.);
#2416=VECTOR('',#8498,1.);
#2417=VECTOR('',#8499,1.);
#2418=VECTOR('',#8500,1.);
#2419=VECTOR('',#8503,1.);
#2420=VECTOR('',#8504,1.);
#2421=VECTOR('',#8505,1.);
#2422=VECTOR('',#8508,1.);
#2423=VECTOR('',#8509,1.);
#2424=VECTOR('',#8510,1.);
#2425=VECTOR('',#8513,1.);
#2426=VECTOR('',#8514,1.);
#2427=VECTOR('',#8515,1.);
#2428=VECTOR('',#8518,1.);
#2429=VECTOR('',#8519,1.);
#2430=VECTOR('',#8520,1.);
#2431=VECTOR('',#8523,1.);
#2432=VECTOR('',#8524,1.);
#2433=VECTOR('',#8525,1.);
#2434=VECTOR('',#8528,1.);
#2435=VECTOR('',#8529,1.);
#2436=VECTOR('',#8530,1.);
#2437=VECTOR('',#8533,1.);
#2438=VECTOR('',#8534,1.);
#2439=VECTOR('',#8573,1.);
#2440=VECTOR('',#8574,1.);
#2441=VECTOR('',#8575,1.);
#2442=VECTOR('',#8576,1.);
#2443=VECTOR('',#8577,1.);
#2444=VECTOR('',#8578,1.);
#2445=VECTOR('',#8579,1.);
#2446=VECTOR('',#8580,1.);
#2447=VECTOR('',#8581,1.);
#2448=VECTOR('',#8582,1.);
#2449=VECTOR('',#8585,1.);
#2450=VECTOR('',#8586,1.);
#2451=VECTOR('',#8587,1.);
#2452=VECTOR('',#8588,1.);
#2453=VECTOR('',#8589,1.);
#2454=VECTOR('',#8590,1.);
#2455=VECTOR('',#8591,1.);
#2456=VECTOR('',#8592,1.);
#2457=VECTOR('',#8593,1.);
#2458=VECTOR('',#8594,1.);
#2459=VECTOR('',#8601,1.);
#2460=VECTOR('',#8602,1.);
#2461=VECTOR('',#8603,1.);
#2462=VECTOR('',#8604,1.);
#2463=VECTOR('',#8607,1.);
#2464=VECTOR('',#8608,1.);
#2465=VECTOR('',#8609,1.);
#2466=VECTOR('',#8612,1.);
#2467=VECTOR('',#8613,1.);
#2468=VECTOR('',#8614,1.);
#2469=VECTOR('',#8617,1.);
#2470=VECTOR('',#8618,1.);
#2471=VECTOR('',#8619,1.);
#2472=VECTOR('',#8622,1.);
#2473=VECTOR('',#8623,1.);
#2474=VECTOR('',#8624,1.);
#2475=VECTOR('',#8627,1.);
#2476=VECTOR('',#8628,1.);
#2477=VECTOR('',#8629,1.);
#2478=VECTOR('',#8632,1.);
#2479=VECTOR('',#8633,1.);
#2480=VECTOR('',#8634,1.);
#2481=VECTOR('',#8637,1.);
#2482=VECTOR('',#8638,1.);
#2483=VECTOR('',#8639,1.);
#2484=VECTOR('',#8642,1.);
#2485=VECTOR('',#8643,1.);
#2486=VECTOR('',#8646,1.);
#2487=VECTOR('',#8647,1.);
#2488=VECTOR('',#8650,1.);
#2489=VECTOR('',#8651,1.);
#2490=VECTOR('',#8654,1.);
#2491=VECTOR('',#8655,1.);
#2492=VECTOR('',#8658,1.);
#2493=VECTOR('',#8659,1.);
#2494=VECTOR('',#8662,1.);
#2495=VECTOR('',#8663,1.);
#2496=VECTOR('',#8666,1.);
#2497=VECTOR('',#8667,1.);
#2498=VECTOR('',#8670,1.);
#2499=VECTOR('',#8671,1.);
#2500=VECTOR('',#8674,1.);
#2501=VECTOR('',#8675,1.);
#2502=VECTOR('',#8678,1.);
#2503=VECTOR('',#8715,1.);
#2504=VECTOR('',#8716,1.);
#2505=VECTOR('',#8717,1.);
#2506=VECTOR('',#8718,1.);
#2507=VECTOR('',#8721,1.);
#2508=VECTOR('',#8722,1.);
#2509=VECTOR('',#8723,1.);
#2510=VECTOR('',#8726,1.);
#2511=VECTOR('',#8727,1.);
#2512=VECTOR('',#8728,1.);
#2513=VECTOR('',#8731,1.);
#2514=VECTOR('',#8732,1.);
#2515=VECTOR('',#8733,1.);
#2516=VECTOR('',#8736,1.);
#2517=VECTOR('',#8737,1.);
#2518=VECTOR('',#8738,1.);
#2519=VECTOR('',#8741,1.);
#2520=VECTOR('',#8742,1.);
#2521=VECTOR('',#8743,1.);
#2522=VECTOR('',#8746,1.);
#2523=VECTOR('',#8747,1.);
#2524=VECTOR('',#8748,1.);
#2525=VECTOR('',#8751,1.);
#2526=VECTOR('',#8752,1.);
#2527=VECTOR('',#8753,1.);
#2528=VECTOR('',#8756,1.);
#2529=VECTOR('',#8757,1.);
#2530=VECTOR('',#8760,1.);
#2531=VECTOR('',#8761,1.);
#2532=VECTOR('',#8764,1.);
#2533=VECTOR('',#8765,1.);
#2534=VECTOR('',#8768,1.);
#2535=VECTOR('',#8769,1.);
#2536=VECTOR('',#8772,1.);
#2537=VECTOR('',#8773,1.);
#2538=VECTOR('',#8776,1.);
#2539=VECTOR('',#8777,1.);
#2540=VECTOR('',#8780,1.);
#2541=VECTOR('',#8781,1.);
#2542=VECTOR('',#8784,1.);
#2543=VECTOR('',#8785,1.);
#2544=VECTOR('',#8788,1.);
#2545=VECTOR('',#8789,1.);
#2546=VECTOR('',#8792,1.);
#2547=VECTOR('',#8831,1.37);
#2548=VECTOR('',#8838,0.21);
#2549=VECTOR('',#8843,0.6);
#2550=VECTOR('',#8848,1.);
#2551=VECTOR('',#8849,1.);
#2552=VECTOR('',#8850,1.);
#2553=VECTOR('',#8851,1.);
#2554=VECTOR('',#8854,1.);
#2555=VECTOR('',#8855,1.);
#2556=VECTOR('',#8856,1.);
#2557=VECTOR('',#8859,1.);
#2558=VECTOR('',#8860,1.);
#2559=VECTOR('',#8861,1.);
#2560=VECTOR('',#8864,1.);
#2561=VECTOR('',#8865,1.);
#2562=VECTOR('',#8866,1.);
#2563=VECTOR('',#8869,1.);
#2564=VECTOR('',#8870,1.);
#2565=VECTOR('',#8871,1.);
#2566=VECTOR('',#8874,1.);
#2567=VECTOR('',#8875,1.);
#2568=VECTOR('',#8876,1.);
#2569=VECTOR('',#8879,1.);
#2570=VECTOR('',#8880,1.);
#2571=VECTOR('',#8881,1.);
#2572=VECTOR('',#8884,1.);
#2573=VECTOR('',#8885,1.);
#2574=VECTOR('',#8886,1.);
#2575=VECTOR('',#8889,1.);
#2576=VECTOR('',#8890,1.);
#2577=VECTOR('',#8891,1.);
#2578=VECTOR('',#8894,1.);
#2579=VECTOR('',#8895,1.);
#2580=VECTOR('',#8896,1.);
#2581=VECTOR('',#8899,1.);
#2582=VECTOR('',#8900,1.);
#2583=VECTOR('',#8901,1.);
#2584=VECTOR('',#8904,1.);
#2585=VECTOR('',#8905,1.);
#2586=VECTOR('',#8906,1.);
#2587=VECTOR('',#8909,1.);
#2588=VECTOR('',#8910,1.);
#2589=VECTOR('',#8911,1.);
#2590=VECTOR('',#8914,1.);
#2591=VECTOR('',#8915,1.);
#2592=VECTOR('',#8916,1.);
#2593=VECTOR('',#8919,1.);
#2594=VECTOR('',#8920,1.);
#2595=VECTOR('',#8921,1.);
#2596=VECTOR('',#8924,1.);
#2597=VECTOR('',#8925,1.);
#2598=VECTOR('',#8926,1.);
#2599=VECTOR('',#8929,1.);
#2600=VECTOR('',#8930,1.);
#2601=VECTOR('',#8931,1.);
#2602=VECTOR('',#8934,1.);
#2603=VECTOR('',#8935,1.);
#2604=VECTOR('',#8968,1.);
#2605=VECTOR('',#8969,1.);
#2606=VECTOR('',#8970,1.);
#2607=VECTOR('',#8971,1.);
#2608=VECTOR('',#8972,1.);
#2609=VECTOR('',#8973,1.);
#2610=VECTOR('',#8974,1.);
#2611=VECTOR('',#8975,1.);
#2612=VECTOR('',#8976,1.);
#2613=VECTOR('',#8977,1.);
#2614=VECTOR('',#8980,1.);
#2615=VECTOR('',#8981,1.);
#2616=VECTOR('',#8982,1.);
#2617=VECTOR('',#8983,1.);
#2618=VECTOR('',#8984,1.);
#2619=VECTOR('',#8985,1.);
#2620=VECTOR('',#8986,1.);
#2621=VECTOR('',#8987,1.);
#2622=VECTOR('',#8988,1.);
#2623=VECTOR('',#8989,1.);
#2624=VECTOR('',#9002,1.);
#2625=VECTOR('',#9003,1.);
#2626=VECTOR('',#9004,1.);
#2627=VECTOR('',#9007,1.);
#2628=VECTOR('',#9008,1.);
#2629=VECTOR('',#9011,1.);
#2630=VECTOR('',#9012,1.);
#2631=VECTOR('',#9015,1.);
#2632=VECTOR('',#9016,1.);
#2633=VECTOR('',#9019,1.);
#2634=VECTOR('',#9020,1.);
#2635=VECTOR('',#9023,1.);
#2636=VECTOR('',#9024,1.);
#2637=VECTOR('',#9027,1.);
#2638=VECTOR('',#9028,1.);
#2639=VECTOR('',#9031,1.);
#2640=VECTOR('',#9032,1.);
#2641=VECTOR('',#9035,1.);
#2642=VECTOR('',#9036,1.);
#2643=VECTOR('',#9039,1.);
#2644=VECTOR('',#9040,1.);
#2645=VECTOR('',#9041,1.);
#2646=VECTOR('',#9044,1.);
#2647=VECTOR('',#9045,1.);
#2648=VECTOR('',#9046,1.);
#2649=VECTOR('',#9049,1.);
#2650=VECTOR('',#9050,1.);
#2651=VECTOR('',#9051,1.);
#2652=VECTOR('',#9054,1.);
#2653=VECTOR('',#9055,1.);
#2654=VECTOR('',#9056,1.);
#2655=VECTOR('',#9059,1.);
#2656=VECTOR('',#9060,1.);
#2657=VECTOR('',#9061,1.);
#2658=VECTOR('',#9064,1.);
#2659=VECTOR('',#9065,1.);
#2660=VECTOR('',#9066,1.);
#2661=VECTOR('',#9069,1.);
#2662=VECTOR('',#9070,1.);
#2663=VECTOR('',#9071,1.);
#2664=VECTOR('',#9074,1.);
#2665=VECTOR('',#9075,1.);
#2666=VECTOR('',#9076,1.);
#2667=VECTOR('',#9079,1.);
#2668=VECTOR('',#9116,1.);
#2669=VECTOR('',#9117,1.);
#2670=VECTOR('',#9118,1.);
#2671=VECTOR('',#9121,1.);
#2672=VECTOR('',#9122,1.);
#2673=VECTOR('',#9125,1.);
#2674=VECTOR('',#9126,1.);
#2675=VECTOR('',#9129,1.);
#2676=VECTOR('',#9130,1.);
#2677=VECTOR('',#9133,1.);
#2678=VECTOR('',#9134,1.);
#2679=VECTOR('',#9137,1.);
#2680=VECTOR('',#9138,1.);
#2681=VECTOR('',#9141,1.);
#2682=VECTOR('',#9142,1.);
#2683=VECTOR('',#9145,1.);
#2684=VECTOR('',#9146,1.);
#2685=VECTOR('',#9149,1.);
#2686=VECTOR('',#9150,1.);
#2687=VECTOR('',#9153,1.);
#2688=VECTOR('',#9154,1.);
#2689=VECTOR('',#9155,1.);
#2690=VECTOR('',#9158,1.);
#2691=VECTOR('',#9159,1.);
#2692=VECTOR('',#9160,1.);
#2693=VECTOR('',#9163,1.);
#2694=VECTOR('',#9164,1.);
#2695=VECTOR('',#9165,1.);
#2696=VECTOR('',#9168,1.);
#2697=VECTOR('',#9169,1.);
#2698=VECTOR('',#9170,1.);
#2699=VECTOR('',#9173,1.);
#2700=VECTOR('',#9174,1.);
#2701=VECTOR('',#9175,1.);
#2702=VECTOR('',#9178,1.);
#2703=VECTOR('',#9179,1.);
#2704=VECTOR('',#9180,1.);
#2705=VECTOR('',#9183,1.);
#2706=VECTOR('',#9184,1.);
#2707=VECTOR('',#9185,1.);
#2708=VECTOR('',#9188,1.);
#2709=VECTOR('',#9189,1.);
#2710=VECTOR('',#9190,1.);
#2711=VECTOR('',#9193,1.);
#2712=VECTOR('',#9232,1.37);
#2713=VECTOR('',#9239,1.);
#2714=VECTOR('',#9240,1.);
#2715=VECTOR('',#9241,1.);
#2716=VECTOR('',#9242,1.);
#2717=VECTOR('',#9243,1.);
#2718=VECTOR('',#9244,1.);
#2719=VECTOR('',#9245,1.);
#2720=VECTOR('',#9246,1.);
#2721=VECTOR('',#9249,1.);
#2722=VECTOR('',#9250,1.);
#2723=VECTOR('',#9251,1.);
#2724=VECTOR('',#9252,1.);
#2725=VECTOR('',#9253,1.);
#2726=VECTOR('',#9254,1.);
#2727=VECTOR('',#9255,1.);
#2728=VECTOR('',#9256,1.);
#2729=VECTOR('',#9259,1.);
#2730=VECTOR('',#9260,1.);
#2731=VECTOR('',#9261,1.);
#2732=VECTOR('',#9262,1.);
#2733=VECTOR('',#9263,1.);
#2734=VECTOR('',#9264,1.);
#2735=VECTOR('',#9265,1.);
#2736=VECTOR('',#9266,1.);
#2737=VECTOR('',#9269,1.);
#2738=VECTOR('',#9270,1.);
#2739=VECTOR('',#9271,1.);
#2740=VECTOR('',#9272,1.);
#2741=VECTOR('',#9273,1.);
#2742=VECTOR('',#9274,1.);
#2743=VECTOR('',#9275,1.);
#2744=VECTOR('',#9276,1.);
#2745=VECTOR('',#9279,1.);
#2746=VECTOR('',#9280,1.);
#2747=VECTOR('',#9281,1.);
#2748=VECTOR('',#9282,1.);
#2749=VECTOR('',#9283,1.);
#2750=VECTOR('',#9284,1.);
#2751=VECTOR('',#9285,1.);
#2752=VECTOR('',#9286,1.);
#2753=VECTOR('',#9289,1.);
#2754=VECTOR('',#9290,1.);
#2755=VECTOR('',#9291,1.);
#2756=VECTOR('',#9292,1.);
#2757=VECTOR('',#9293,1.);
#2758=VECTOR('',#9294,1.);
#2759=VECTOR('',#9295,1.);
#2760=VECTOR('',#9296,1.);
#2761=VECTOR('',#9301,1.);
#2762=VECTOR('',#9304,1.);
#2763=VECTOR('',#9307,1.);
#2764=VECTOR('',#9310,1.);
#2765=VECTOR('',#9313,1.);
#2766=VECTOR('',#9316,1.);
#2767=VECTOR('',#9319,1.);
#2768=VECTOR('',#9320,1.);
#2769=VECTOR('',#9325,1.);
#2770=VECTOR('',#9326,1.);
#2771=VECTOR('',#9331,1.);
#2772=VECTOR('',#9332,1.);
#2773=VECTOR('',#9337,1.);
#2774=VECTOR('',#9338,1.);
#2775=VECTOR('',#9339,1.);
#2776=VECTOR('',#9340,1.);
#2777=VECTOR('',#9341,1.);
#2778=VECTOR('',#9342,1.);
#2779=VECTOR('',#9343,1.);
#2780=VECTOR('',#9344,1.);
#2781=VECTOR('',#9345,1.);
#2782=VECTOR('',#9346,1.);
#2783=VECTOR('',#9347,1.);
#2784=VECTOR('',#9348,1.);
#2785=VECTOR('',#9349,1.);
#2786=VECTOR('',#9350,1.);
#2787=VECTOR('',#9351,1.);
#2788=VECTOR('',#9352,1.);
#2789=VECTOR('',#9353,1.);
#2790=VECTOR('',#9354,1.);
#2791=VECTOR('',#9355,1.);
#2792=VECTOR('',#9356,1.);
#2793=VECTOR('',#9357,1.);
#2794=VECTOR('',#9358,1.);
#2795=VECTOR('',#9359,1.);
#2796=VECTOR('',#9360,1.);
#2797=VECTOR('',#9361,1.);
#2798=VECTOR('',#9362,1.);
#2799=VECTOR('',#9363,1.);
#2800=VECTOR('',#9364,1.);
#2801=VECTOR('',#9365,1.);
#2802=VECTOR('',#9366,1.);
#2803=VECTOR('',#9367,1.);
#2804=VECTOR('',#9368,1.);
#2805=VECTOR('',#9369,1.);
#2806=VECTOR('',#9370,1.);
#2807=VECTOR('',#9371,1.);
#2808=VECTOR('',#9372,1.);
#2809=VECTOR('',#9373,1.);
#2810=VECTOR('',#9374,1.);
#2811=VECTOR('',#9375,1.);
#2812=VECTOR('',#9376,1.);
#2813=VECTOR('',#9377,1.);
#2814=VECTOR('',#9378,1.);
#2815=VECTOR('',#9379,1.);
#2816=VECTOR('',#9380,1.);
#2817=VECTOR('',#9381,1.);
#2818=VECTOR('',#9382,1.);
#2819=VECTOR('',#9383,1.);
#2820=VECTOR('',#9384,1.);
#2821=VECTOR('',#9387,1.);
#2822=VECTOR('',#9388,1.);
#2823=VECTOR('',#9389,1.);
#2824=VECTOR('',#9390,1.);
#2825=VECTOR('',#9391,1.);
#2826=VECTOR('',#9394,1.);
#2827=VECTOR('',#9395,1.);
#2828=VECTOR('',#9398,1.);
#2829=VECTOR('',#9399,1.);
#2830=VECTOR('',#9402,1.);
#2831=VECTOR('',#9403,1.);
#2832=VECTOR('',#9406,1.);
#2833=VECTOR('',#9407,1.);
#2834=VECTOR('',#9410,1.);
#2835=VECTOR('',#9411,1.);
#2836=VECTOR('',#9414,1.);
#2837=VECTOR('',#9415,1.);
#2838=VECTOR('',#9418,1.);
#2839=VECTOR('',#9419,1.);
#2840=VECTOR('',#9422,1.);
#2841=VECTOR('',#9423,1.);
#2842=VECTOR('',#9424,1.);
#2843=VECTOR('',#9425,1.);
#2844=VECTOR('',#9426,1.);
#2845=VECTOR('',#9427,1.);
#2846=VECTOR('',#9428,1.);
#2847=VECTOR('',#9429,1.);
#2848=VECTOR('',#9430,1.);
#2849=VECTOR('',#9431,1.);
#2850=VECTOR('',#9432,1.);
#2851=VECTOR('',#9433,1.);
#2852=VECTOR('',#9436,1.);
#2853=VECTOR('',#9437,1.);
#2854=VECTOR('',#9440,1.);
#2855=VECTOR('',#9443,1.);
#2856=VECTOR('',#9446,1.);
#2857=VECTOR('',#9451,1.);
#2858=VECTOR('',#9452,1.);
#2859=VECTOR('',#9455,1.);
#2860=VECTOR('',#9456,1.);
#2861=VECTOR('',#9459,1.);
#2862=VECTOR('',#9460,1.);
#2863=VECTOR('',#9463,1.);
#2864=VECTOR('',#9464,1.);
#2865=VECTOR('',#9467,1.);
#2866=VECTOR('',#9468,1.);
#2867=VECTOR('',#9471,1.);
#2868=VECTOR('',#9472,1.);
#2869=VECTOR('',#9475,1.);
#2870=VECTOR('',#9480,1.);
#2871=VECTOR('',#9481,1.);
#2872=VECTOR('',#9482,1.);
#2873=VECTOR('',#9483,1.);
#2874=VECTOR('',#9484,1.);
#2875=VECTOR('',#9487,1.);
#2876=VECTOR('',#9488,1.);
#2877=VECTOR('',#9491,1.);
#2878=VECTOR('',#9492,1.);
#2879=VECTOR('',#9495,1.);
#2880=VECTOR('',#9496,1.);
#2881=VECTOR('',#9499,1.);
#2882=VECTOR('',#9500,1.);
#2883=VECTOR('',#9503,1.);
#2884=VECTOR('',#9504,1.);
#2885=VECTOR('',#9507,1.);
#2886=VECTOR('',#9508,1.);
#2887=VECTOR('',#9511,1.);
#2888=VECTOR('',#9512,1.);
#2889=VECTOR('',#9515,1.);
#2890=VECTOR('',#9516,1.);
#2891=VECTOR('',#9517,1.);
#2892=VECTOR('',#9518,1.);
#2893=VECTOR('',#9519,1.);
#2894=VECTOR('',#9520,1.);
#2895=VECTOR('',#9521,1.);
#2896=VECTOR('',#9522,1.);
#2897=VECTOR('',#9523,1.);
#2898=VECTOR('',#9524,1.);
#2899=VECTOR('',#9525,1.);
#2900=VECTOR('',#9526,1.);
#2901=VECTOR('',#9529,1.);
#2902=VECTOR('',#9530,1.);
#2903=VECTOR('',#9533,1.);
#2904=VECTOR('',#9536,1.);
#2905=VECTOR('',#9539,1.);
#2906=VECTOR('',#9544,1.);
#2907=VECTOR('',#9545,1.);
#2908=VECTOR('',#9548,1.);
#2909=VECTOR('',#9549,1.);
#2910=VECTOR('',#9552,1.);
#2911=VECTOR('',#9553,1.);
#2912=VECTOR('',#9556,1.);
#2913=VECTOR('',#9557,1.);
#2914=VECTOR('',#9560,1.);
#2915=VECTOR('',#9561,1.);
#2916=VECTOR('',#9564,1.);
#2917=VECTOR('',#9565,1.);
#2918=VECTOR('',#9568,1.);
#2919=VECTOR('',#9573,1.);
#2920=VECTOR('',#9574,1.);
#2921=VECTOR('',#9575,1.);
#2922=VECTOR('',#9576,1.);
#2923=VECTOR('',#9577,1.);
#2924=VECTOR('',#9580,1.);
#2925=VECTOR('',#9581,1.);
#2926=VECTOR('',#9584,1.);
#2927=VECTOR('',#9585,1.);
#2928=VECTOR('',#9588,1.);
#2929=VECTOR('',#9589,1.);
#2930=VECTOR('',#9592,1.);
#2931=VECTOR('',#9593,1.);
#2932=VECTOR('',#9596,1.);
#2933=VECTOR('',#9597,1.);
#2934=VECTOR('',#9600,1.);
#2935=VECTOR('',#9601,1.);
#2936=VECTOR('',#9604,1.);
#2937=VECTOR('',#9605,1.);
#2938=VECTOR('',#9608,1.);
#2939=VECTOR('',#9609,1.);
#2940=VECTOR('',#9610,1.);
#2941=VECTOR('',#9611,1.);
#2942=VECTOR('',#9612,1.);
#2943=VECTOR('',#9613,1.);
#2944=VECTOR('',#9614,1.);
#2945=VECTOR('',#9615,1.);
#2946=VECTOR('',#9616,1.);
#2947=VECTOR('',#9617,1.);
#2948=VECTOR('',#9618,1.);
#2949=VECTOR('',#9619,1.);
#2950=VECTOR('',#9622,1.);
#2951=VECTOR('',#9623,1.);
#2952=VECTOR('',#9626,1.);
#2953=VECTOR('',#9629,1.);
#2954=VECTOR('',#9632,1.);
#2955=VECTOR('',#9637,1.);
#2956=VECTOR('',#9638,1.);
#2957=VECTOR('',#9641,1.);
#2958=VECTOR('',#9642,1.);
#2959=VECTOR('',#9645,1.);
#2960=VECTOR('',#9646,1.);
#2961=VECTOR('',#9649,1.);
#2962=VECTOR('',#9650,1.);
#2963=VECTOR('',#9653,1.);
#2964=VECTOR('',#9654,1.);
#2965=VECTOR('',#9657,1.);
#2966=VECTOR('',#9658,1.);
#2967=VECTOR('',#9661,1.);
#2968=VECTOR('',#9666,1.);
#2969=VECTOR('',#9667,1.);
#2970=VECTOR('',#9668,1.);
#2971=VECTOR('',#9669,1.);
#2972=VECTOR('',#9670,1.);
#2973=VECTOR('',#9673,1.);
#2974=VECTOR('',#9674,1.);
#2975=VECTOR('',#9677,1.);
#2976=VECTOR('',#9678,1.);
#2977=VECTOR('',#9681,1.);
#2978=VECTOR('',#9682,1.);
#2979=VECTOR('',#9685,1.);
#2980=VECTOR('',#9686,1.);
#2981=VECTOR('',#9689,1.);
#2982=VECTOR('',#9690,1.);
#2983=VECTOR('',#9693,1.);
#2984=VECTOR('',#9694,1.);
#2985=VECTOR('',#9697,1.);
#2986=VECTOR('',#9698,1.);
#2987=VECTOR('',#9701,1.);
#2988=VECTOR('',#9702,1.);
#2989=VECTOR('',#9703,1.);
#2990=VECTOR('',#9704,1.);
#2991=VECTOR('',#9705,1.);
#2992=VECTOR('',#9706,1.);
#2993=VECTOR('',#9707,1.);
#2994=VECTOR('',#9708,1.);
#2995=VECTOR('',#9709,1.);
#2996=VECTOR('',#9710,1.);
#2997=VECTOR('',#9711,1.);
#2998=VECTOR('',#9712,1.);
#2999=VECTOR('',#9715,1.);
#3000=VECTOR('',#9716,1.);
#3001=VECTOR('',#9719,1.);
#3002=VECTOR('',#9722,1.);
#3003=VECTOR('',#9725,1.);
#3004=VECTOR('',#9730,1.);
#3005=VECTOR('',#9731,1.);
#3006=VECTOR('',#9734,1.);
#3007=VECTOR('',#9735,1.);
#3008=VECTOR('',#9738,1.);
#3009=VECTOR('',#9739,1.);
#3010=VECTOR('',#9742,1.);
#3011=VECTOR('',#9743,1.);
#3012=VECTOR('',#9746,1.);
#3013=VECTOR('',#9747,1.);
#3014=VECTOR('',#9750,1.);
#3015=VECTOR('',#9751,1.);
#3016=VECTOR('',#9754,1.);
#3017=VECTOR('',#9759,1.);
#3018=VECTOR('',#9760,1.);
#3019=VECTOR('',#9761,1.);
#3020=VECTOR('',#9762,1.);
#3021=VECTOR('',#9763,1.);
#3022=VECTOR('',#9766,1.);
#3023=VECTOR('',#9767,1.);
#3024=VECTOR('',#9770,1.);
#3025=VECTOR('',#9771,1.);
#3026=VECTOR('',#9774,1.);
#3027=VECTOR('',#9775,1.);
#3028=VECTOR('',#9778,1.);
#3029=VECTOR('',#9779,1.);
#3030=VECTOR('',#9782,1.);
#3031=VECTOR('',#9783,1.);
#3032=VECTOR('',#9786,1.);
#3033=VECTOR('',#9787,1.);
#3034=VECTOR('',#9790,1.);
#3035=VECTOR('',#9791,1.);
#3036=VECTOR('',#9794,1.);
#3037=VECTOR('',#9795,1.);
#3038=VECTOR('',#9796,1.);
#3039=VECTOR('',#9797,1.);
#3040=VECTOR('',#9798,1.);
#3041=VECTOR('',#9799,1.);
#3042=VECTOR('',#9800,1.);
#3043=VECTOR('',#9801,1.);
#3044=VECTOR('',#9802,1.);
#3045=VECTOR('',#9803,1.);
#3046=VECTOR('',#9804,1.);
#3047=VECTOR('',#9805,1.);
#3048=VECTOR('',#9808,1.);
#3049=VECTOR('',#9809,1.);
#3050=VECTOR('',#9812,1.);
#3051=VECTOR('',#9815,1.);
#3052=VECTOR('',#9818,1.);
#3053=VECTOR('',#9823,1.);
#3054=VECTOR('',#9824,1.);
#3055=VECTOR('',#9827,1.);
#3056=VECTOR('',#9828,1.);
#3057=VECTOR('',#9831,1.);
#3058=VECTOR('',#9832,1.);
#3059=VECTOR('',#9835,1.);
#3060=VECTOR('',#9836,1.);
#3061=VECTOR('',#9839,1.);
#3062=VECTOR('',#9840,1.);
#3063=VECTOR('',#9843,1.);
#3064=VECTOR('',#9844,1.);
#3065=VECTOR('',#9847,1.);
#3066=VECTOR('',#9852,1.);
#3067=VECTOR('',#9853,1.);
#3068=VECTOR('',#9854,1.);
#3069=VECTOR('',#9855,1.);
#3070=VECTOR('',#9856,1.);
#3071=VECTOR('',#9859,1.);
#3072=VECTOR('',#9860,1.);
#3073=VECTOR('',#9863,1.);
#3074=VECTOR('',#9864,1.);
#3075=VECTOR('',#9867,1.);
#3076=VECTOR('',#9868,1.);
#3077=VECTOR('',#9871,1.);
#3078=VECTOR('',#9872,1.);
#3079=VECTOR('',#9875,1.);
#3080=VECTOR('',#9876,1.);
#3081=VECTOR('',#9879,1.);
#3082=VECTOR('',#9880,1.);
#3083=VECTOR('',#9883,1.);
#3084=VECTOR('',#9884,1.);
#3085=VECTOR('',#9887,1.);
#3086=VECTOR('',#9888,1.);
#3087=VECTOR('',#9889,1.);
#3088=VECTOR('',#9890,1.);
#3089=VECTOR('',#9891,1.);
#3090=VECTOR('',#9892,1.);
#3091=VECTOR('',#9893,1.);
#3092=VECTOR('',#9894,1.);
#3093=VECTOR('',#9895,1.);
#3094=VECTOR('',#9896,1.);
#3095=VECTOR('',#9897,1.);
#3096=VECTOR('',#9898,1.);
#3097=VECTOR('',#9901,1.);
#3098=VECTOR('',#9902,1.);
#3099=VECTOR('',#9905,1.);
#3100=VECTOR('',#9908,1.);
#3101=VECTOR('',#9911,1.);
#3102=VECTOR('',#9916,1.);
#3103=VECTOR('',#9917,1.);
#3104=VECTOR('',#9920,1.);
#3105=VECTOR('',#9921,1.);
#3106=VECTOR('',#9924,1.);
#3107=VECTOR('',#9925,1.);
#3108=VECTOR('',#9928,1.);
#3109=VECTOR('',#9929,1.);
#3110=VECTOR('',#9932,1.);
#3111=VECTOR('',#9933,1.);
#3112=VECTOR('',#9936,1.);
#3113=VECTOR('',#9937,1.);
#3114=VECTOR('',#9940,1.);
#3115=VECTOR('',#9953,1.);
#3116=VECTOR('',#9954,1.);
#3117=VECTOR('',#9955,1.);
#3118=VECTOR('',#9956,1.);
#3119=VECTOR('',#9959,1.);
#3120=VECTOR('',#9960,1.);
#3121=VECTOR('',#9961,1.);
#3122=VECTOR('',#9964,1.);
#3123=VECTOR('',#9965,1.);
#3124=VECTOR('',#9966,1.);
#3125=VECTOR('',#9969,1.);
#3126=VECTOR('',#9970,1.);
#3127=VECTOR('',#9971,1.);
#3128=VECTOR('',#9974,1.);
#3129=VECTOR('',#9975,1.);
#3130=VECTOR('',#9976,1.);
#3131=VECTOR('',#9979,1.);
#3132=VECTOR('',#9980,1.);
#3133=VECTOR('',#9991,0.235);
#3134=VECTOR('',#9996,0.25);
#3135=VECTOR('',#10001,0.2125);
#3136=CIRCLE('',#7485,0.21);
#3137=CIRCLE('',#7486,0.21);
#3138=CIRCLE('',#7488,0.21);
#3139=CIRCLE('',#7489,0.21);
#3140=CIRCLE('',#7491,0.21);
#3141=CIRCLE('',#7492,0.21);
#3142=CIRCLE('',#7494,0.21);
#3143=CIRCLE('',#7495,0.21);
#3144=CIRCLE('',#7504,0.6);
#3145=CIRCLE('',#7505,0.6);
#3146=CIRCLE('',#7510,0.6);
#3147=CIRCLE('',#7511,0.6);
#3148=CIRCLE('',#7516,0.525);
#3149=CIRCLE('',#7518,0.525);
#3150=CIRCLE('',#7520,0.525);
#3151=CIRCLE('',#7521,0.525);
#3152=CIRCLE('',#7524,0.275);
#3153=CIRCLE('',#7526,0.165);
#3154=CIRCLE('',#7528,0.275);
#3155=CIRCLE('',#7530,0.225);
#3156=CIRCLE('',#7531,0.225);
#3157=CIRCLE('',#7533,0.165);
#3158=CIRCLE('',#7535,0.275);
#3159=CIRCLE('',#7537,0.275);
#3160=CIRCLE('',#7539,0.6);
#3161=CIRCLE('',#7540,0.6);
#3162=CIRCLE('',#7562,0.24505);
#3163=CIRCLE('',#7564,0.375);
#3164=CIRCLE('',#7566,0.425);
#3165=CIRCLE('',#7568,0.425);
#3166=CIRCLE('',#7570,0.395);
#3167=CIRCLE('',#7572,0.27);
#3168=CIRCLE('',#7574,0.24505);
#3169=CIRCLE('',#7578,0.3);
#3170=CIRCLE('',#7580,0.35);
#3171=CIRCLE('',#7582,0.35);
#3172=CIRCLE('',#7584,0.32);
#3173=CIRCLE('',#7586,0.22);
#3174=CIRCLE('',#7588,0.1954);
#3175=CIRCLE('',#7590,0.1954);
#3176=CIRCLE('',#7592,0.16);
#3177=CIRCLE('',#7605,1.05);
#3178=CIRCLE('',#7606,0.6);
#3179=CIRCLE('',#7608,1.1);
#3180=CIRCLE('',#7610,1.1);
#3181=CIRCLE('',#7612,1.05);
#3182=CIRCLE('',#7614,0.6);
#3183=CIRCLE('',#7620,0.6);
#3184=CIRCLE('',#7621,0.6);
#3185=CIRCLE('',#7642,1.37);
#3186=CIRCLE('',#7644,1.37);
#3187=CIRCLE('',#7646,1.37);
#3188=CIRCLE('',#7648,1.37);
#3189=CIRCLE('',#7650,1.37);
#3190=CIRCLE('',#7652,1.37);
#3191=CIRCLE('',#7654,1.37);
#3192=CIRCLE('',#7656,1.37);
#3193=CIRCLE('',#7658,1.37);
#3194=CIRCLE('',#7659,1.37);
#3195=CIRCLE('',#7660,1.37);
#3196=CIRCLE('',#7661,1.37);
#3197=CIRCLE('',#7682,1.37);
#3198=CIRCLE('',#7684,1.37);
#3199=CIRCLE('',#7686,1.37);
#3200=CIRCLE('',#7688,1.37);
#3201=CIRCLE('',#7690,1.37);
#3202=CIRCLE('',#7692,1.37);
#3203=CIRCLE('',#7694,1.37);
#3204=CIRCLE('',#7696,1.37);
#3205=CIRCLE('',#7717,1.37);
#3206=CIRCLE('',#7719,1.37);
#3207=CIRCLE('',#7721,1.37);
#3208=CIRCLE('',#7723,1.37);
#3209=CIRCLE('',#7725,1.37);
#3210=CIRCLE('',#7727,1.37);
#3211=CIRCLE('',#7729,1.37);
#3212=CIRCLE('',#7731,1.37);
#3213=CIRCLE('',#7733,1.37);
#3214=CIRCLE('',#7738,0.6);
#3215=CIRCLE('',#7739,0.6);
#3216=CIRCLE('',#7760,1.37);
#3217=CIRCLE('',#7762,1.37);
#3218=CIRCLE('',#7764,1.37);
#3219=CIRCLE('',#7766,1.37);
#3220=CIRCLE('',#7768,1.37);
#3221=CIRCLE('',#7770,1.37);
#3222=CIRCLE('',#7772,1.37);
#3223=CIRCLE('',#7773,1.37);
#3224=CIRCLE('',#7774,1.37);
#3225=CIRCLE('',#7775,1.37);
#3226=CIRCLE('',#7777,1.37);
#3227=CIRCLE('',#7779,1.37);
#3228=CIRCLE('',#7800,1.37);
#3229=CIRCLE('',#7802,1.37);
#3230=CIRCLE('',#7804,1.37);
#3231=CIRCLE('',#7806,1.37);
#3232=CIRCLE('',#7808,1.37);
#3233=CIRCLE('',#7810,1.37);
#3234=CIRCLE('',#7812,1.37);
#3235=CIRCLE('',#7814,1.37);
#3236=CIRCLE('',#7835,1.37);
#3237=CIRCLE('',#7837,1.37);
#3238=CIRCLE('',#7839,1.37);
#3239=CIRCLE('',#7841,1.37);
#3240=CIRCLE('',#7843,1.37);
#3241=CIRCLE('',#7845,1.37);
#3242=CIRCLE('',#7847,1.37);
#3243=CIRCLE('',#7849,1.37);
#3244=CIRCLE('',#7851,1.37);
#3245=CIRCLE('',#7855,0.817);
#3246=CIRCLE('',#7856,0.817);
#3247=CIRCLE('',#7857,0.817);
#3248=CIRCLE('',#7858,0.817);
#3249=CIRCLE('',#7859,0.817);
#3250=CIRCLE('',#7860,0.817);
#3251=CIRCLE('',#7862,0.817);
#3252=CIRCLE('',#7864,0.817);
#3253=CIRCLE('',#7866,0.817);
#3254=CIRCLE('',#7868,0.817);
#3255=CIRCLE('',#7870,0.817);
#3256=CIRCLE('',#7872,0.817);
#3257=CIRCLE('',#8018,0.22);
#3258=CIRCLE('',#8020,0.24505);
#3259=CIRCLE('',#8022,0.24505);
#3260=CIRCLE('',#8024,0.175);
#3261=VERTEX_POINT('',#10043);
#3262=VERTEX_POINT('',#10045);
#3263=VERTEX_POINT('',#10049);
#3264=VERTEX_POINT('',#10051);
#3265=VERTEX_POINT('',#10055);
#3266=VERTEX_POINT('',#10057);
#3267=VERTEX_POINT('',#10061);
#3268=VERTEX_POINT('',#10063);
#3269=VERTEX_POINT('',#10067);
#3270=VERTEX_POINT('',#10068);
#3271=VERTEX_POINT('',#10070);
#3272=VERTEX_POINT('',#10072);
#3273=VERTEX_POINT('',#10076);
#3274=VERTEX_POINT('',#10078);
#3275=VERTEX_POINT('',#10082);
#3276=VERTEX_POINT('',#10084);
#3277=VERTEX_POINT('',#10094);
#3278=VERTEX_POINT('',#10096);
#3279=VERTEX_POINT('',#10103);
#3280=VERTEX_POINT('',#10105);
#3281=VERTEX_POINT('',#10112);
#3282=VERTEX_POINT('',#10113);
#3283=VERTEX_POINT('',#10117);
#3284=VERTEX_POINT('',#10119);
#3285=VERTEX_POINT('',#10123);
#3286=VERTEX_POINT('',#10124);
#3287=VERTEX_POINT('',#10126);
#3288=VERTEX_POINT('',#10128);
#3289=VERTEX_POINT('',#10134);
#3290=VERTEX_POINT('',#10136);
#3291=VERTEX_POINT('',#10138);
#3292=VERTEX_POINT('',#10140);
#3293=VERTEX_POINT('',#10143);
#3294=VERTEX_POINT('',#10146);
#3295=VERTEX_POINT('',#10148);
#3296=VERTEX_POINT('',#10151);
#3297=VERTEX_POINT('',#10154);
#3298=VERTEX_POINT('',#10155);
#3299=VERTEX_POINT('',#10157);
#3300=VERTEX_POINT('',#10160);
#3301=VERTEX_POINT('',#10163);
#3302=VERTEX_POINT('',#10166);
#3303=VERTEX_POINT('',#10168);
#3304=VERTEX_POINT('',#10172);
#3305=VERTEX_POINT('',#10176);
#3306=VERTEX_POINT('',#10180);
#3307=VERTEX_POINT('',#10184);
#3308=VERTEX_POINT('',#10186);
#3309=VERTEX_POINT('',#10190);
#3310=VERTEX_POINT('',#10192);
#3311=VERTEX_POINT('',#10195);
#3312=VERTEX_POINT('',#10197);
#3313=VERTEX_POINT('',#10199);
#3314=VERTEX_POINT('',#10201);
#3315=VERTEX_POINT('',#10203);
#3316=VERTEX_POINT('',#10207);
#3317=VERTEX_POINT('',#10211);
#3318=VERTEX_POINT('',#10217);
#3319=VERTEX_POINT('',#10221);
#3320=VERTEX_POINT('',#10225);
#3321=VERTEX_POINT('',#10229);
#3322=VERTEX_POINT('',#10233);
#3323=VERTEX_POINT('',#10241);
#3324=VERTEX_POINT('',#10242);
#3325=VERTEX_POINT('',#10244);
#3326=VERTEX_POINT('',#10246);
#3327=VERTEX_POINT('',#10250);
#3328=VERTEX_POINT('',#10252);
#3329=VERTEX_POINT('',#10256);
#3330=VERTEX_POINT('',#10258);
#3331=VERTEX_POINT('',#10262);
#3332=VERTEX_POINT('',#10264);
#3333=VERTEX_POINT('',#10268);
#3334=VERTEX_POINT('',#10270);
#3335=VERTEX_POINT('',#10279);
#3336=VERTEX_POINT('',#10282);
#3337=VERTEX_POINT('',#10285);
#3338=VERTEX_POINT('',#10289);
#3339=VERTEX_POINT('',#10293);
#3340=VERTEX_POINT('',#10297);
#3341=VERTEX_POINT('',#10300);
#3342=VERTEX_POINT('',#10307);
#3343=VERTEX_POINT('',#10310);
#3344=VERTEX_POINT('',#10314);
#3345=VERTEX_POINT('',#10318);
#3346=VERTEX_POINT('',#10322);
#3347=VERTEX_POINT('',#10325);
#3348=VERTEX_POINT('',#10329);
#3349=VERTEX_POINT('',#10333);
#3350=VERTEX_POINT('',#10338);
#3351=VERTEX_POINT('',#10339);
#3352=VERTEX_POINT('',#10341);
#3353=VERTEX_POINT('',#10343);
#3354=VERTEX_POINT('',#10347);
#3355=VERTEX_POINT('',#10349);
#3356=VERTEX_POINT('',#10353);
#3357=VERTEX_POINT('',#10355);
#3358=VERTEX_POINT('',#10359);
#3359=VERTEX_POINT('',#10361);
#3360=VERTEX_POINT('',#10365);
#3361=VERTEX_POINT('',#10367);
#3362=VERTEX_POINT('',#10377);
#3363=VERTEX_POINT('',#10412);
#3364=VERTEX_POINT('',#10449);
#3365=VERTEX_POINT('',#10451);
#3366=VERTEX_POINT('',#10454);
#3367=VERTEX_POINT('',#10458);
#3368=VERTEX_POINT('',#10462);
#3369=VERTEX_POINT('',#10466);
#3370=VERTEX_POINT('',#10473);
#3371=VERTEX_POINT('',#10474);
#3372=VERTEX_POINT('',#10511);
#3373=VERTEX_POINT('',#10548);
#3374=VERTEX_POINT('',#10550);
#3375=VERTEX_POINT('',#10554);
#3376=VERTEX_POINT('',#10555);
#3377=VERTEX_POINT('',#10557);
#3378=VERTEX_POINT('',#10559);
#3379=VERTEX_POINT('',#10563);
#3380=VERTEX_POINT('',#10565);
#3381=VERTEX_POINT('',#10569);
#3382=VERTEX_POINT('',#10571);
#3383=VERTEX_POINT('',#10575);
#3384=VERTEX_POINT('',#10577);
#3385=VERTEX_POINT('',#10581);
#3386=VERTEX_POINT('',#10583);
#3387=VERTEX_POINT('',#10587);
#3388=VERTEX_POINT('',#10589);
#3389=VERTEX_POINT('',#10593);
#3390=VERTEX_POINT('',#10595);
#3391=VERTEX_POINT('',#10599);
#3392=VERTEX_POINT('',#10601);
#3393=VERTEX_POINT('',#10605);
#3394=VERTEX_POINT('',#10607);
#3395=VERTEX_POINT('',#10611);
#3396=VERTEX_POINT('',#10613);
#3397=VERTEX_POINT('',#10617);
#3398=VERTEX_POINT('',#10619);
#3399=VERTEX_POINT('',#10623);
#3400=VERTEX_POINT('',#10625);
#3401=VERTEX_POINT('',#10629);
#3402=VERTEX_POINT('',#10631);
#3403=VERTEX_POINT('',#10635);
#3404=VERTEX_POINT('',#10637);
#3405=VERTEX_POINT('',#10641);
#3406=VERTEX_POINT('',#10643);
#3407=VERTEX_POINT('',#10647);
#3408=VERTEX_POINT('',#10649);
#3409=VERTEX_POINT('',#10653);
#3410=VERTEX_POINT('',#10655);
#3411=VERTEX_POINT('',#10679);
#3412=VERTEX_POINT('',#10681);
#3413=VERTEX_POINT('',#10683);
#3414=VERTEX_POINT('',#10685);
#3415=VERTEX_POINT('',#10687);
#3416=VERTEX_POINT('',#10689);
#3417=VERTEX_POINT('',#10691);
#3418=VERTEX_POINT('',#10693);
#3419=VERTEX_POINT('',#10695);
#3420=VERTEX_POINT('',#10697);
#3421=VERTEX_POINT('',#10699);
#3422=VERTEX_POINT('',#10701);
#3423=VERTEX_POINT('',#10703);
#3424=VERTEX_POINT('',#10705);
#3425=VERTEX_POINT('',#10707);
#3426=VERTEX_POINT('',#10709);
#3427=VERTEX_POINT('',#10711);
#3428=VERTEX_POINT('',#10713);
#3429=VERTEX_POINT('',#10715);
#3430=VERTEX_POINT('',#10717);
#3431=VERTEX_POINT('',#10719);
#3432=VERTEX_POINT('',#10721);
#3433=VERTEX_POINT('',#10723);
#3434=VERTEX_POINT('',#10727);
#3435=VERTEX_POINT('',#10728);
#3436=VERTEX_POINT('',#10731);
#3437=VERTEX_POINT('',#10735);
#3438=VERTEX_POINT('',#10737);
#3439=VERTEX_POINT('',#10741);
#3440=VERTEX_POINT('',#10743);
#3441=VERTEX_POINT('',#10747);
#3442=VERTEX_POINT('',#10749);
#3443=VERTEX_POINT('',#10753);
#3444=VERTEX_POINT('',#10755);
#3445=VERTEX_POINT('',#10759);
#3446=VERTEX_POINT('',#10761);
#3447=VERTEX_POINT('',#10765);
#3448=VERTEX_POINT('',#10767);
#3449=VERTEX_POINT('',#10771);
#3450=VERTEX_POINT('',#10776);
#3451=VERTEX_POINT('',#10780);
#3452=VERTEX_POINT('',#10784);
#3453=VERTEX_POINT('',#10788);
#3454=VERTEX_POINT('',#10792);
#3455=VERTEX_POINT('',#10796);
#3456=VERTEX_POINT('',#10800);
#3457=VERTEX_POINT('',#10804);
#3458=VERTEX_POINT('',#10808);
#3459=VERTEX_POINT('',#10831);
#3460=VERTEX_POINT('',#10832);
#3461=VERTEX_POINT('',#10835);
#3462=VERTEX_POINT('',#10839);
#3463=VERTEX_POINT('',#10841);
#3464=VERTEX_POINT('',#10845);
#3465=VERTEX_POINT('',#10847);
#3466=VERTEX_POINT('',#10851);
#3467=VERTEX_POINT('',#10853);
#3468=VERTEX_POINT('',#10857);
#3469=VERTEX_POINT('',#10859);
#3470=VERTEX_POINT('',#10863);
#3471=VERTEX_POINT('',#10865);
#3472=VERTEX_POINT('',#10869);
#3473=VERTEX_POINT('',#10871);
#3474=VERTEX_POINT('',#10875);
#3475=VERTEX_POINT('',#10880);
#3476=VERTEX_POINT('',#10884);
#3477=VERTEX_POINT('',#10888);
#3478=VERTEX_POINT('',#10892);
#3479=VERTEX_POINT('',#10896);
#3480=VERTEX_POINT('',#10900);
#3481=VERTEX_POINT('',#10904);
#3482=VERTEX_POINT('',#10908);
#3483=VERTEX_POINT('',#10912);
#3484=VERTEX_POINT('',#10935);
#3485=VERTEX_POINT('',#10941);
#3486=VERTEX_POINT('',#10942);
#3487=VERTEX_POINT('',#10979);
#3488=VERTEX_POINT('',#10981);
#3489=VERTEX_POINT('',#11019);
#3490=VERTEX_POINT('',#11021);
#3491=VERTEX_POINT('',#11025);
#3492=VERTEX_POINT('',#11026);
#3493=VERTEX_POINT('',#11028);
#3494=VERTEX_POINT('',#11030);
#3495=VERTEX_POINT('',#11034);
#3496=VERTEX_POINT('',#11036);
#3497=VERTEX_POINT('',#11040);
#3498=VERTEX_POINT('',#11042);
#3499=VERTEX_POINT('',#11046);
#3500=VERTEX_POINT('',#11048);
#3501=VERTEX_POINT('',#11052);
#3502=VERTEX_POINT('',#11054);
#3503=VERTEX_POINT('',#11058);
#3504=VERTEX_POINT('',#11060);
#3505=VERTEX_POINT('',#11064);
#3506=VERTEX_POINT('',#11066);
#3507=VERTEX_POINT('',#11070);
#3508=VERTEX_POINT('',#11072);
#3509=VERTEX_POINT('',#11076);
#3510=VERTEX_POINT('',#11078);
#3511=VERTEX_POINT('',#11082);
#3512=VERTEX_POINT('',#11084);
#3513=VERTEX_POINT('',#11088);
#3514=VERTEX_POINT('',#11090);
#3515=VERTEX_POINT('',#11094);
#3516=VERTEX_POINT('',#11096);
#3517=VERTEX_POINT('',#11100);
#3518=VERTEX_POINT('',#11102);
#3519=VERTEX_POINT('',#11106);
#3520=VERTEX_POINT('',#11108);
#3521=VERTEX_POINT('',#11112);
#3522=VERTEX_POINT('',#11114);
#3523=VERTEX_POINT('',#11118);
#3524=VERTEX_POINT('',#11120);
#3525=VERTEX_POINT('',#11124);
#3526=VERTEX_POINT('',#11126);
#3527=VERTEX_POINT('',#11146);
#3528=VERTEX_POINT('',#11148);
#3529=VERTEX_POINT('',#11150);
#3530=VERTEX_POINT('',#11152);
#3531=VERTEX_POINT('',#11154);
#3532=VERTEX_POINT('',#11156);
#3533=VERTEX_POINT('',#11158);
#3534=VERTEX_POINT('',#11160);
#3535=VERTEX_POINT('',#11162);
#3536=VERTEX_POINT('',#11164);
#3537=VERTEX_POINT('',#11166);
#3538=VERTEX_POINT('',#11168);
#3539=VERTEX_POINT('',#11170);
#3540=VERTEX_POINT('',#11172);
#3541=VERTEX_POINT('',#11174);
#3542=VERTEX_POINT('',#11176);
#3543=VERTEX_POINT('',#11178);
#3544=VERTEX_POINT('',#11180);
#3545=VERTEX_POINT('',#11182);
#3546=VERTEX_POINT('',#11184);
#3547=VERTEX_POINT('',#11186);
#3548=VERTEX_POINT('',#11188);
#3549=VERTEX_POINT('',#11190);
#3550=VERTEX_POINT('',#11198);
#3551=VERTEX_POINT('',#11199);
#3552=VERTEX_POINT('',#11204);
#3553=VERTEX_POINT('',#11208);
#3554=VERTEX_POINT('',#11212);
#3555=VERTEX_POINT('',#11216);
#3556=VERTEX_POINT('',#11220);
#3557=VERTEX_POINT('',#11224);
#3558=VERTEX_POINT('',#11228);
#3559=VERTEX_POINT('',#11232);
#3560=VERTEX_POINT('',#11236);
#3561=VERTEX_POINT('',#11238);
#3562=VERTEX_POINT('',#11242);
#3563=VERTEX_POINT('',#11244);
#3564=VERTEX_POINT('',#11248);
#3565=VERTEX_POINT('',#11250);
#3566=VERTEX_POINT('',#11254);
#3567=VERTEX_POINT('',#11256);
#3568=VERTEX_POINT('',#11260);
#3569=VERTEX_POINT('',#11262);
#3570=VERTEX_POINT('',#11266);
#3571=VERTEX_POINT('',#11268);
#3572=VERTEX_POINT('',#11272);
#3573=VERTEX_POINT('',#11274);
#3574=VERTEX_POINT('',#11278);
#3575=VERTEX_POINT('',#11302);
#3576=VERTEX_POINT('',#11303);
#3577=VERTEX_POINT('',#11308);
#3578=VERTEX_POINT('',#11312);
#3579=VERTEX_POINT('',#11316);
#3580=VERTEX_POINT('',#11320);
#3581=VERTEX_POINT('',#11324);
#3582=VERTEX_POINT('',#11328);
#3583=VERTEX_POINT('',#11332);
#3584=VERTEX_POINT('',#11336);
#3585=VERTEX_POINT('',#11340);
#3586=VERTEX_POINT('',#11342);
#3587=VERTEX_POINT('',#11346);
#3588=VERTEX_POINT('',#11348);
#3589=VERTEX_POINT('',#11352);
#3590=VERTEX_POINT('',#11354);
#3591=VERTEX_POINT('',#11358);
#3592=VERTEX_POINT('',#11360);
#3593=VERTEX_POINT('',#11364);
#3594=VERTEX_POINT('',#11366);
#3595=VERTEX_POINT('',#11370);
#3596=VERTEX_POINT('',#11372);
#3597=VERTEX_POINT('',#11376);
#3598=VERTEX_POINT('',#11378);
#3599=VERTEX_POINT('',#11382);
#3600=VERTEX_POINT('',#11406);
#3601=VERTEX_POINT('',#11412);
#3602=VERTEX_POINT('',#11413);
#3603=VERTEX_POINT('',#11415);
#3604=VERTEX_POINT('',#11417);
#3605=VERTEX_POINT('',#11419);
#3606=VERTEX_POINT('',#11421);
#3607=VERTEX_POINT('',#11423);
#3608=VERTEX_POINT('',#11425);
#3609=VERTEX_POINT('',#11427);
#3610=VERTEX_POINT('',#11429);
#3611=VERTEX_POINT('',#11431);
#3612=VERTEX_POINT('',#11433);
#3613=VERTEX_POINT('',#11435);
#3614=VERTEX_POINT('',#11437);
#3615=VERTEX_POINT('',#11439);
#3616=VERTEX_POINT('',#11441);
#3617=VERTEX_POINT('',#11443);
#3618=VERTEX_POINT('',#11445);
#3619=VERTEX_POINT('',#11447);
#3620=VERTEX_POINT('',#11449);
#3621=VERTEX_POINT('',#11451);
#3622=VERTEX_POINT('',#11453);
#3623=VERTEX_POINT('',#11455);
#3624=VERTEX_POINT('',#11457);
#3625=VERTEX_POINT('',#11459);
#3626=VERTEX_POINT('',#11461);
#3627=VERTEX_POINT('',#11463);
#3628=VERTEX_POINT('',#11465);
#3629=VERTEX_POINT('',#11467);
#3630=VERTEX_POINT('',#11469);
#3631=VERTEX_POINT('',#11471);
#3632=VERTEX_POINT('',#11473);
#3633=VERTEX_POINT('',#11475);
#3634=VERTEX_POINT('',#11477);
#3635=VERTEX_POINT('',#11479);
#3636=VERTEX_POINT('',#11481);
#3637=VERTEX_POINT('',#11483);
#3638=VERTEX_POINT('',#11485);
#3639=VERTEX_POINT('',#11487);
#3640=VERTEX_POINT('',#11489);
#3641=VERTEX_POINT('',#11491);
#3642=VERTEX_POINT('',#11493);
#3643=VERTEX_POINT('',#11495);
#3644=VERTEX_POINT('',#11497);
#3645=VERTEX_POINT('',#11499);
#3646=VERTEX_POINT('',#11501);
#3647=VERTEX_POINT('',#11503);
#3648=VERTEX_POINT('',#11505);
#3649=VERTEX_POINT('',#11507);
#3650=VERTEX_POINT('',#11509);
#3651=VERTEX_POINT('',#11511);
#3652=VERTEX_POINT('',#11513);
#3653=VERTEX_POINT('',#11515);
#3654=VERTEX_POINT('',#11517);
#3655=VERTEX_POINT('',#11521);
#3656=VERTEX_POINT('',#11523);
#3657=VERTEX_POINT('',#11527);
#3658=VERTEX_POINT('',#11529);
#3659=VERTEX_POINT('',#11533);
#3660=VERTEX_POINT('',#11535);
#3661=VERTEX_POINT('',#11539);
#3662=VERTEX_POINT('',#11541);
#3663=VERTEX_POINT('',#11545);
#3664=VERTEX_POINT('',#11547);
#3665=VERTEX_POINT('',#11551);
#3666=VERTEX_POINT('',#11553);
#3667=VERTEX_POINT('',#11557);
#3668=VERTEX_POINT('',#11559);
#3669=VERTEX_POINT('',#11561);
#3670=VERTEX_POINT('',#11563);
#3671=VERTEX_POINT('',#11565);
#3672=VERTEX_POINT('',#11567);
#3673=VERTEX_POINT('',#11569);
#3674=VERTEX_POINT('',#11571);
#3675=VERTEX_POINT('',#11574);
#3676=VERTEX_POINT('',#11576);
#3677=VERTEX_POINT('',#11578);
#3678=VERTEX_POINT('',#11580);
#3679=VERTEX_POINT('',#11582);
#3680=VERTEX_POINT('',#11584);
#3681=VERTEX_POINT('',#11586);
#3682=VERTEX_POINT('',#11589);
#3683=VERTEX_POINT('',#11591);
#3684=VERTEX_POINT('',#11593);
#3685=VERTEX_POINT('',#11595);
#3686=VERTEX_POINT('',#11597);
#3687=VERTEX_POINT('',#11599);
#3688=VERTEX_POINT('',#11601);
#3689=VERTEX_POINT('',#11604);
#3690=VERTEX_POINT('',#11606);
#3691=VERTEX_POINT('',#11608);
#3692=VERTEX_POINT('',#11610);
#3693=VERTEX_POINT('',#11612);
#3694=VERTEX_POINT('',#11614);
#3695=VERTEX_POINT('',#11616);
#3696=VERTEX_POINT('',#11619);
#3697=VERTEX_POINT('',#11621);
#3698=VERTEX_POINT('',#11623);
#3699=VERTEX_POINT('',#11625);
#3700=VERTEX_POINT('',#11627);
#3701=VERTEX_POINT('',#11629);
#3702=VERTEX_POINT('',#11631);
#3703=VERTEX_POINT('',#11634);
#3704=VERTEX_POINT('',#11636);
#3705=VERTEX_POINT('',#11638);
#3706=VERTEX_POINT('',#11640);
#3707=VERTEX_POINT('',#11642);
#3708=VERTEX_POINT('',#11644);
#3709=VERTEX_POINT('',#11648);
#3710=VERTEX_POINT('',#11650);
#3711=VERTEX_POINT('',#11652);
#3712=VERTEX_POINT('',#11654);
#3713=VERTEX_POINT('',#11658);
#3714=VERTEX_POINT('',#11662);
#3715=VERTEX_POINT('',#11666);
#3716=VERTEX_POINT('',#11670);
#3717=VERTEX_POINT('',#11674);
#3718=VERTEX_POINT('',#11678);
#3719=VERTEX_POINT('',#11682);
#3720=VERTEX_POINT('',#11686);
#3721=VERTEX_POINT('',#11687);
#3722=VERTEX_POINT('',#11689);
#3723=VERTEX_POINT('',#11691);
#3724=VERTEX_POINT('',#11693);
#3725=VERTEX_POINT('',#11695);
#3726=VERTEX_POINT('',#11698);
#3727=VERTEX_POINT('',#11700);
#3728=VERTEX_POINT('',#11702);
#3729=VERTEX_POINT('',#11704);
#3730=VERTEX_POINT('',#11706);
#3731=VERTEX_POINT('',#11720);
#3732=VERTEX_POINT('',#11724);
#3733=VERTEX_POINT('',#11728);
#3734=VERTEX_POINT('',#11732);
#3735=VERTEX_POINT('',#11736);
#3736=VERTEX_POINT('',#11740);
#3737=VERTEX_POINT('',#11747);
#3738=VERTEX_POINT('',#11749);
#3739=VERTEX_POINT('',#11751);
#3740=VERTEX_POINT('',#11753);
#3741=VERTEX_POINT('',#11757);
#3742=VERTEX_POINT('',#11761);
#3743=VERTEX_POINT('',#11765);
#3744=VERTEX_POINT('',#11769);
#3745=VERTEX_POINT('',#11773);
#3746=VERTEX_POINT('',#11777);
#3747=VERTEX_POINT('',#11781);
#3748=VERTEX_POINT('',#11785);
#3749=VERTEX_POINT('',#11786);
#3750=VERTEX_POINT('',#11788);
#3751=VERTEX_POINT('',#11790);
#3752=VERTEX_POINT('',#11792);
#3753=VERTEX_POINT('',#11794);
#3754=VERTEX_POINT('',#11797);
#3755=VERTEX_POINT('',#11799);
#3756=VERTEX_POINT('',#11801);
#3757=VERTEX_POINT('',#11803);
#3758=VERTEX_POINT('',#11805);
#3759=VERTEX_POINT('',#11819);
#3760=VERTEX_POINT('',#11823);
#3761=VERTEX_POINT('',#11827);
#3762=VERTEX_POINT('',#11831);
#3763=VERTEX_POINT('',#11835);
#3764=VERTEX_POINT('',#11839);
#3765=VERTEX_POINT('',#11846);
#3766=VERTEX_POINT('',#11848);
#3767=VERTEX_POINT('',#11850);
#3768=VERTEX_POINT('',#11852);
#3769=VERTEX_POINT('',#11856);
#3770=VERTEX_POINT('',#11860);
#3771=VERTEX_POINT('',#11864);
#3772=VERTEX_POINT('',#11868);
#3773=VERTEX_POINT('',#11872);
#3774=VERTEX_POINT('',#11876);
#3775=VERTEX_POINT('',#11880);
#3776=VERTEX_POINT('',#11884);
#3777=VERTEX_POINT('',#11885);
#3778=VERTEX_POINT('',#11887);
#3779=VERTEX_POINT('',#11889);
#3780=VERTEX_POINT('',#11891);
#3781=VERTEX_POINT('',#11893);
#3782=VERTEX_POINT('',#11896);
#3783=VERTEX_POINT('',#11898);
#3784=VERTEX_POINT('',#11900);
#3785=VERTEX_POINT('',#11902);
#3786=VERTEX_POINT('',#11904);
#3787=VERTEX_POINT('',#11918);
#3788=VERTEX_POINT('',#11922);
#3789=VERTEX_POINT('',#11926);
#3790=VERTEX_POINT('',#11930);
#3791=VERTEX_POINT('',#11934);
#3792=VERTEX_POINT('',#11938);
#3793=VERTEX_POINT('',#11945);
#3794=VERTEX_POINT('',#11947);
#3795=VERTEX_POINT('',#11949);
#3796=VERTEX_POINT('',#11951);
#3797=VERTEX_POINT('',#11955);
#3798=VERTEX_POINT('',#11959);
#3799=VERTEX_POINT('',#11963);
#3800=VERTEX_POINT('',#11967);
#3801=VERTEX_POINT('',#11971);
#3802=VERTEX_POINT('',#11975);
#3803=VERTEX_POINT('',#11979);
#3804=VERTEX_POINT('',#11983);
#3805=VERTEX_POINT('',#11984);
#3806=VERTEX_POINT('',#11986);
#3807=VERTEX_POINT('',#11988);
#3808=VERTEX_POINT('',#11990);
#3809=VERTEX_POINT('',#11992);
#3810=VERTEX_POINT('',#11995);
#3811=VERTEX_POINT('',#11997);
#3812=VERTEX_POINT('',#11999);
#3813=VERTEX_POINT('',#12001);
#3814=VERTEX_POINT('',#12003);
#3815=VERTEX_POINT('',#12017);
#3816=VERTEX_POINT('',#12021);
#3817=VERTEX_POINT('',#12025);
#3818=VERTEX_POINT('',#12029);
#3819=VERTEX_POINT('',#12033);
#3820=VERTEX_POINT('',#12037);
#3821=VERTEX_POINT('',#12044);
#3822=VERTEX_POINT('',#12046);
#3823=VERTEX_POINT('',#12048);
#3824=VERTEX_POINT('',#12050);
#3825=VERTEX_POINT('',#12054);
#3826=VERTEX_POINT('',#12058);
#3827=VERTEX_POINT('',#12062);
#3828=VERTEX_POINT('',#12066);
#3829=VERTEX_POINT('',#12070);
#3830=VERTEX_POINT('',#12074);
#3831=VERTEX_POINT('',#12078);
#3832=VERTEX_POINT('',#12082);
#3833=VERTEX_POINT('',#12083);
#3834=VERTEX_POINT('',#12085);
#3835=VERTEX_POINT('',#12087);
#3836=VERTEX_POINT('',#12089);
#3837=VERTEX_POINT('',#12091);
#3838=VERTEX_POINT('',#12094);
#3839=VERTEX_POINT('',#12096);
#3840=VERTEX_POINT('',#12098);
#3841=VERTEX_POINT('',#12100);
#3842=VERTEX_POINT('',#12102);
#3843=VERTEX_POINT('',#12116);
#3844=VERTEX_POINT('',#12120);
#3845=VERTEX_POINT('',#12124);
#3846=VERTEX_POINT('',#12128);
#3847=VERTEX_POINT('',#12132);
#3848=VERTEX_POINT('',#12136);
#3849=VERTEX_POINT('',#12143);
#3850=VERTEX_POINT('',#12145);
#3851=VERTEX_POINT('',#12147);
#3852=VERTEX_POINT('',#12149);
#3853=VERTEX_POINT('',#12153);
#3854=VERTEX_POINT('',#12157);
#3855=VERTEX_POINT('',#12161);
#3856=VERTEX_POINT('',#12165);
#3857=VERTEX_POINT('',#12169);
#3858=VERTEX_POINT('',#12173);
#3859=VERTEX_POINT('',#12177);
#3860=VERTEX_POINT('',#12181);
#3861=VERTEX_POINT('',#12182);
#3862=VERTEX_POINT('',#12184);
#3863=VERTEX_POINT('',#12186);
#3864=VERTEX_POINT('',#12188);
#3865=VERTEX_POINT('',#12190);
#3866=VERTEX_POINT('',#12193);
#3867=VERTEX_POINT('',#12195);
#3868=VERTEX_POINT('',#12197);
#3869=VERTEX_POINT('',#12199);
#3870=VERTEX_POINT('',#12201);
#3871=VERTEX_POINT('',#12215);
#3872=VERTEX_POINT('',#12219);
#3873=VERTEX_POINT('',#12223);
#3874=VERTEX_POINT('',#12227);
#3875=VERTEX_POINT('',#12231);
#3876=VERTEX_POINT('',#12235);
#3877=VERTEX_POINT('',#12246);
#3878=VERTEX_POINT('',#12247);
#3879=VERTEX_POINT('',#12249);
#3880=VERTEX_POINT('',#12251);
#3881=VERTEX_POINT('',#12255);
#3882=VERTEX_POINT('',#12257);
#3883=VERTEX_POINT('',#12261);
#3884=VERTEX_POINT('',#12263);
#3885=VERTEX_POINT('',#12267);
#3886=VERTEX_POINT('',#12269);
#3887=VERTEX_POINT('',#12273);
#3888=VERTEX_POINT('',#12275);
#3889=VERTEX_POINT('',#12283);
#3890=VERTEX_POINT('',#12286);
#3891=VERTEX_POINT('',#12290);
#3892=VERTEX_POINT('',#12294);
#3893=EDGE_CURVE('',#3261,#3261,#3136,.T.);
#3894=EDGE_CURVE('',#3261,#3262,#1392,.T.);
#3895=EDGE_CURVE('',#3262,#3262,#3137,.T.);
#3896=EDGE_CURVE('',#3263,#3263,#3138,.T.);
#3897=EDGE_CURVE('',#3263,#3264,#1393,.T.);
#3898=EDGE_CURVE('',#3264,#3264,#3139,.T.);
#3899=EDGE_CURVE('',#3265,#3265,#3140,.T.);
#3900=EDGE_CURVE('',#3265,#3266,#1394,.T.);
#3901=EDGE_CURVE('',#3266,#3266,#3141,.T.);
#3902=EDGE_CURVE('',#3267,#3267,#3142,.T.);
#3903=EDGE_CURVE('',#3267,#3268,#1395,.T.);
#3904=EDGE_CURVE('',#3268,#3268,#3143,.T.);
#3905=EDGE_CURVE('',#3269,#3270,#1396,.T.);
#3906=EDGE_CURVE('',#3270,#3271,#1397,.T.);
#3907=EDGE_CURVE('',#3272,#3271,#1398,.T.);
#3908=EDGE_CURVE('',#3269,#3272,#1399,.T.);
#3909=EDGE_CURVE('',#3273,#3269,#1400,.T.);
#3910=EDGE_CURVE('',#3274,#3272,#1401,.T.);
#3911=EDGE_CURVE('',#3273,#3274,#1402,.T.);
#3912=EDGE_CURVE('',#3275,#3273,#1403,.T.);
#3913=EDGE_CURVE('',#3276,#3274,#1404,.T.);
#3914=EDGE_CURVE('',#3275,#3276,#1405,.T.);
#3915=EDGE_CURVE('',#3270,#3275,#1406,.T.);
#3916=EDGE_CURVE('',#3271,#3276,#1407,.T.);
#3917=EDGE_CURVE('',#3277,#3277,#3144,.T.);
#3918=EDGE_CURVE('',#3277,#3278,#1408,.T.);
#3919=EDGE_CURVE('',#3278,#3278,#3145,.T.);
#3920=EDGE_CURVE('',#3279,#3279,#3146,.T.);
#3921=EDGE_CURVE('',#3279,#3280,#1409,.T.);
#3922=EDGE_CURVE('',#3280,#3280,#3147,.T.);
#3923=EDGE_CURVE('',#3281,#3282,#1410,.T.);
#3924=EDGE_CURVE('',#3282,#3281,#3148,.T.);
#3925=EDGE_CURVE('',#3283,#3281,#1411,.T.);
#3926=EDGE_CURVE('',#3284,#3283,#3149,.T.);
#3927=EDGE_CURVE('',#3282,#3284,#1412,.T.);
#3928=EDGE_CURVE('',#3285,#3286,#1413,.T.);
#3929=EDGE_CURVE('',#3285,#3287,#3150,.T.);
#3930=EDGE_CURVE('',#3288,#3287,#1414,.T.);
#3931=EDGE_CURVE('',#3286,#3288,#3151,.T.);
#3932=EDGE_CURVE('',#3287,#3285,#1415,.T.);
#3933=EDGE_CURVE('',#3283,#3289,#1416,.T.);
#3934=EDGE_CURVE('',#3290,#3289,#1417,.T.);
#3935=EDGE_CURVE('',#3290,#3291,#1418,.T.);
#3936=EDGE_CURVE('',#3292,#3291,#1419,.T.);
#3937=EDGE_CURVE('',#3292,#3284,#1420,.T.);
#3938=EDGE_CURVE('',#3293,#3293,#3152,.T.);
#3939=EDGE_CURVE('',#3294,#3292,#1421,.T.);
#3940=EDGE_CURVE('',#3294,#3295,#1422,.T.);
#3941=EDGE_CURVE('',#3289,#3295,#1423,.T.);
#3942=EDGE_CURVE('',#3296,#3296,#3153,.T.);
#3943=EDGE_CURVE('',#3297,#3298,#1424,.T.);
#3944=EDGE_CURVE('',#3299,#3298,#1425,.T.);
#3945=EDGE_CURVE('',#3286,#3299,#1426,.T.);
#3946=EDGE_CURVE('',#3300,#3288,#1427,.T.);
#3947=EDGE_CURVE('',#3297,#3300,#1428,.T.);
#3948=EDGE_CURVE('',#3301,#3301,#3154,.T.);
#3949=EDGE_CURVE('',#3302,#3302,#3155,.T.);
#3950=EDGE_CURVE('',#3302,#3303,#1429,.T.);
#3951=EDGE_CURVE('',#3303,#3303,#3156,.T.);
#3952=EDGE_CURVE('',#3296,#3304,#1430,.T.);
#3953=EDGE_CURVE('',#3304,#3304,#3157,.T.);
#3954=EDGE_CURVE('',#3305,#3305,#3158,.T.);
#3955=EDGE_CURVE('',#3305,#3293,#1431,.T.);
#3956=EDGE_CURVE('',#3306,#3306,#3159,.T.);
#3957=EDGE_CURVE('',#3306,#3301,#1432,.T.);
#3958=EDGE_CURVE('',#3307,#3307,#3160,.T.);
#3959=EDGE_CURVE('',#3307,#3308,#1433,.T.);
#3960=EDGE_CURVE('',#3308,#3308,#3161,.T.);
#3961=EDGE_CURVE('',#3291,#3309,#1434,.T.);
#3962=EDGE_CURVE('',#3309,#3310,#1435,.T.);
#3963=EDGE_CURVE('',#3310,#3297,#1436,.T.);
#3964=EDGE_CURVE('',#3300,#3311,#1437,.T.);
#3965=EDGE_CURVE('',#3311,#3312,#1438,.T.);
#3966=EDGE_CURVE('',#3312,#3313,#1439,.T.);
#3967=EDGE_CURVE('',#3313,#3314,#1440,.T.);
#3968=EDGE_CURVE('',#3314,#3315,#1441,.T.);
#3969=EDGE_CURVE('',#3315,#3294,#1442,.T.);
#3970=EDGE_CURVE('',#3316,#3290,#1443,.T.);
#3971=EDGE_CURVE('',#3309,#3316,#1444,.T.);
#3972=EDGE_CURVE('',#3317,#3316,#1445,.T.);
#3973=EDGE_CURVE('',#3310,#3317,#1446,.T.);
#3974=EDGE_CURVE('',#3298,#3317,#1447,.T.);
#3975=EDGE_CURVE('',#3318,#3299,#1448,.T.);
#3976=EDGE_CURVE('',#3311,#3318,#1449,.T.);
#3977=EDGE_CURVE('',#3319,#3318,#1450,.T.);
#3978=EDGE_CURVE('',#3312,#3319,#1451,.T.);
#3979=EDGE_CURVE('',#3320,#3319,#1452,.T.);
#3980=EDGE_CURVE('',#3313,#3320,#1453,.T.);
#3981=EDGE_CURVE('',#3321,#3320,#1454,.T.);
#3982=EDGE_CURVE('',#3314,#3321,#1455,.T.);
#3983=EDGE_CURVE('',#3322,#3321,#1456,.T.);
#3984=EDGE_CURVE('',#3315,#3322,#1457,.T.);
#3985=EDGE_CURVE('',#3295,#3322,#1458,.T.);
#3986=EDGE_CURVE('',#3323,#3324,#1459,.T.);
#3987=EDGE_CURVE('',#3324,#3325,#1460,.T.);
#3988=EDGE_CURVE('',#3325,#3326,#1461,.T.);
#3989=EDGE_CURVE('',#3323,#3326,#1462,.T.);
#3990=EDGE_CURVE('',#3324,#3327,#1463,.T.);
#3991=EDGE_CURVE('',#3327,#3328,#1464,.T.);
#3992=EDGE_CURVE('',#3328,#3325,#1465,.T.);
#3993=EDGE_CURVE('',#3327,#3329,#1466,.T.);
#3994=EDGE_CURVE('',#3329,#3330,#1467,.T.);
#3995=EDGE_CURVE('',#3330,#3328,#1468,.T.);
#3996=EDGE_CURVE('',#3329,#3331,#1469,.T.);
#3997=EDGE_CURVE('',#3331,#3332,#1470,.T.);
#3998=EDGE_CURVE('',#3332,#3330,#1471,.T.);
#3999=EDGE_CURVE('',#3331,#3333,#1472,.T.);
#4000=EDGE_CURVE('',#3333,#3334,#1473,.T.);
#4001=EDGE_CURVE('',#3334,#3332,#1474,.T.);
#4002=EDGE_CURVE('',#3333,#3323,#1475,.T.);
#4003=EDGE_CURVE('',#3326,#3334,#1476,.T.);
#4004=EDGE_CURVE('',#3335,#3335,#3162,.T.);
#4005=EDGE_CURVE('',#3336,#3336,#3163,.T.);
#4006=EDGE_CURVE('',#3337,#3337,#3164,.T.);
#4007=EDGE_CURVE('',#3337,#3336,#1477,.T.);
#4008=EDGE_CURVE('',#3338,#3338,#3165,.T.);
#4009=EDGE_CURVE('',#3338,#3337,#1478,.T.);
#4010=EDGE_CURVE('',#3339,#3339,#3166,.T.);
#4011=EDGE_CURVE('',#3339,#3338,#1479,.T.);
#4012=EDGE_CURVE('',#3340,#3340,#3167,.T.);
#4013=EDGE_CURVE('',#3341,#3341,#3168,.F.);
#4014=EDGE_CURVE('',#3341,#3340,#1480,.T.);
#4015=EDGE_CURVE('',#3335,#3341,#1481,.T.);
#4016=EDGE_CURVE('',#3342,#3342,#3169,.T.);
#4017=EDGE_CURVE('',#3343,#3343,#3170,.T.);
#4018=EDGE_CURVE('',#3343,#3342,#1482,.T.);
#4019=EDGE_CURVE('',#3344,#3344,#3171,.T.);
#4020=EDGE_CURVE('',#3344,#3343,#1483,.T.);
#4021=EDGE_CURVE('',#3345,#3345,#3172,.T.);
#4022=EDGE_CURVE('',#3345,#3344,#1484,.T.);
#4023=EDGE_CURVE('',#3346,#3346,#3173,.T.);
#4024=EDGE_CURVE('',#3347,#3347,#3174,.F.);
#4025=EDGE_CURVE('',#3347,#3346,#1485,.T.);
#4026=EDGE_CURVE('',#3348,#3348,#3175,.F.);
#4027=EDGE_CURVE('',#3348,#3347,#1486,.T.);
#4028=EDGE_CURVE('',#3349,#3349,#3176,.T.);
#4029=EDGE_CURVE('',#3349,#3348,#1487,.T.);
#4030=EDGE_CURVE('',#3350,#3351,#1488,.T.);
#4031=EDGE_CURVE('',#3351,#3352,#1489,.T.);
#4032=EDGE_CURVE('',#3352,#3353,#1490,.T.);
#4033=EDGE_CURVE('',#3350,#3353,#1491,.T.);
#4034=EDGE_CURVE('',#3351,#3354,#1492,.T.);
#4035=EDGE_CURVE('',#3354,#3355,#1493,.T.);
#4036=EDGE_CURVE('',#3355,#3352,#1494,.T.);
#4037=EDGE_CURVE('',#3354,#3356,#1495,.T.);
#4038=EDGE_CURVE('',#3356,#3357,#1496,.T.);
#4039=EDGE_CURVE('',#3357,#3355,#1497,.T.);
#4040=EDGE_CURVE('',#3356,#3358,#1498,.T.);
#4041=EDGE_CURVE('',#3358,#3359,#1499,.T.);
#4042=EDGE_CURVE('',#3359,#3357,#1500,.T.);
#4043=EDGE_CURVE('',#3358,#3360,#1501,.T.);
#4044=EDGE_CURVE('',#3360,#3361,#1502,.T.);
#4045=EDGE_CURVE('',#3361,#3359,#1503,.T.);
#4046=EDGE_CURVE('',#3360,#3350,#1504,.T.);
#4047=EDGE_CURVE('',#3353,#3361,#1505,.T.);
#4048=EDGE_CURVE('',#3362,#3362,#95,.T.);
#4049=EDGE_CURVE('',#3362,#3363,#1506,.T.);
#4050=EDGE_CURVE('',#3363,#3363,#96,.T.);
#4051=EDGE_CURVE('',#3364,#3364,#3177,.T.);
#4052=EDGE_CURVE('',#3365,#3365,#3178,.T.);
#4053=EDGE_CURVE('',#3366,#3366,#3179,.T.);
#4054=EDGE_CURVE('',#3366,#3364,#1507,.T.);
#4055=EDGE_CURVE('',#3367,#3367,#3180,.T.);
#4056=EDGE_CURVE('',#3367,#3366,#1508,.T.);
#4057=EDGE_CURVE('',#3368,#3368,#3181,.T.);
#4058=EDGE_CURVE('',#3368,#3367,#1509,.T.);
#4059=EDGE_CURVE('',#3369,#3369,#3182,.T.);
#4060=EDGE_CURVE('',#3369,#3365,#1510,.T.);
#4061=EDGE_CURVE('',#3370,#3371,#97,.T.);
#4062=EDGE_CURVE('',#3371,#3370,#98,.T.);
#4063=EDGE_CURVE('',#3371,#3372,#1511,.T.);
#4064=EDGE_CURVE('',#3372,#3372,#99,.T.);
#4065=EDGE_CURVE('',#3373,#3373,#3183,.T.);
#4066=EDGE_CURVE('',#3373,#3374,#1512,.T.);
#4067=EDGE_CURVE('',#3374,#3374,#3184,.T.);
#4068=EDGE_CURVE('',#3375,#3376,#1513,.T.);
#4069=EDGE_CURVE('',#3375,#3377,#1514,.T.);
#4070=EDGE_CURVE('',#3378,#3377,#1515,.T.);
#4071=EDGE_CURVE('',#3376,#3378,#1516,.T.);
#4072=EDGE_CURVE('',#3376,#3379,#1517,.T.);
#4073=EDGE_CURVE('',#3380,#3378,#1518,.T.);
#4074=EDGE_CURVE('',#3379,#3380,#1519,.T.);
#4075=EDGE_CURVE('',#3379,#3381,#1520,.T.);
#4076=EDGE_CURVE('',#3382,#3380,#1521,.T.);
#4077=EDGE_CURVE('',#3381,#3382,#1522,.T.);
#4078=EDGE_CURVE('',#3381,#3383,#1523,.T.);
#4079=EDGE_CURVE('',#3384,#3382,#1524,.T.);
#4080=EDGE_CURVE('',#3383,#3384,#1525,.T.);
#4081=EDGE_CURVE('',#3383,#3385,#1526,.T.);
#4082=EDGE_CURVE('',#3386,#3384,#1527,.T.);
#4083=EDGE_CURVE('',#3385,#3386,#1528,.T.);
#4084=EDGE_CURVE('',#3385,#3387,#1529,.T.);
#4085=EDGE_CURVE('',#3388,#3386,#1530,.T.);
#4086=EDGE_CURVE('',#3387,#3388,#1531,.T.);
#4087=EDGE_CURVE('',#3387,#3389,#1532,.T.);
#4088=EDGE_CURVE('',#3390,#3388,#1533,.T.);
#4089=EDGE_CURVE('',#3389,#3390,#1534,.T.);
#4090=EDGE_CURVE('',#3389,#3391,#1535,.T.);
#4091=EDGE_CURVE('',#3392,#3390,#1536,.T.);
#4092=EDGE_CURVE('',#3391,#3392,#1537,.T.);
#4093=EDGE_CURVE('',#3391,#3393,#1538,.T.);
#4094=EDGE_CURVE('',#3394,#3392,#1539,.T.);
#4095=EDGE_CURVE('',#3393,#3394,#1540,.T.);
#4096=EDGE_CURVE('',#3393,#3395,#1541,.T.);
#4097=EDGE_CURVE('',#3396,#3394,#1542,.T.);
#4098=EDGE_CURVE('',#3395,#3396,#1543,.T.);
#4099=EDGE_CURVE('',#3395,#3397,#1544,.T.);
#4100=EDGE_CURVE('',#3398,#3396,#1545,.T.);
#4101=EDGE_CURVE('',#3397,#3398,#1546,.T.);
#4102=EDGE_CURVE('',#3397,#3399,#1547,.T.);
#4103=EDGE_CURVE('',#3400,#3398,#1548,.T.);
#4104=EDGE_CURVE('',#3399,#3400,#1549,.T.);
#4105=EDGE_CURVE('',#3399,#3401,#1550,.T.);
#4106=EDGE_CURVE('',#3402,#3400,#1551,.T.);
#4107=EDGE_CURVE('',#3401,#3402,#1552,.T.);
#4108=EDGE_CURVE('',#3401,#3403,#1553,.T.);
#4109=EDGE_CURVE('',#3404,#3402,#1554,.T.);
#4110=EDGE_CURVE('',#3403,#3404,#1555,.T.);
#4111=EDGE_CURVE('',#3403,#3405,#1556,.T.);
#4112=EDGE_CURVE('',#3406,#3404,#1557,.T.);
#4113=EDGE_CURVE('',#3405,#3406,#1558,.T.);
#4114=EDGE_CURVE('',#3405,#3407,#1559,.T.);
#4115=EDGE_CURVE('',#3408,#3406,#1560,.T.);
#4116=EDGE_CURVE('',#3407,#3408,#1561,.T.);
#4117=EDGE_CURVE('',#3407,#3409,#1562,.T.);
#4118=EDGE_CURVE('',#3410,#3408,#1563,.T.);
#4119=EDGE_CURVE('',#3409,#3410,#1564,.T.);
#4120=EDGE_CURVE('',#3409,#3375,#1565,.T.);
#4121=EDGE_CURVE('',#3377,#3410,#1566,.T.);
#4122=EDGE_CURVE('',#3377,#3378,#3185,.T.);
#4123=EDGE_CURVE('',#3378,#3380,#3186,.T.);
#4124=EDGE_CURVE('',#3380,#3382,#3187,.T.);
#4125=EDGE_CURVE('',#3382,#3384,#3188,.T.);
#4126=EDGE_CURVE('',#3384,#3386,#3189,.T.);
#4127=EDGE_CURVE('',#3386,#3388,#3190,.T.);
#4128=EDGE_CURVE('',#3388,#3390,#3191,.T.);
#4129=EDGE_CURVE('',#3390,#3392,#3192,.T.);
#4130=EDGE_CURVE('',#3392,#3411,#3193,.T.);
#4131=EDGE_CURVE('',#3411,#3412,#1567,.T.);
#4132=EDGE_CURVE('',#3412,#3413,#1568,.T.);
#4133=EDGE_CURVE('',#3413,#3414,#1569,.T.);
#4134=EDGE_CURVE('',#3414,#3415,#1570,.T.);
#4135=EDGE_CURVE('',#3415,#3416,#1571,.T.);
#4136=EDGE_CURVE('',#3416,#3417,#1572,.T.);
#4137=EDGE_CURVE('',#3417,#3418,#1573,.T.);
#4138=EDGE_CURVE('',#3418,#3419,#1574,.T.);
#4139=EDGE_CURVE('',#3419,#3420,#1575,.T.);
#4140=EDGE_CURVE('',#3420,#3421,#1576,.T.);
#4141=EDGE_CURVE('',#3421,#3422,#3194,.T.);
#4142=EDGE_CURVE('',#3422,#3423,#1577,.T.);
#4143=EDGE_CURVE('',#3423,#3424,#1578,.T.);
#4144=EDGE_CURVE('',#3424,#3425,#1579,.T.);
#4145=EDGE_CURVE('',#3425,#3426,#1580,.T.);
#4146=EDGE_CURVE('',#3426,#3427,#1581,.T.);
#4147=EDGE_CURVE('',#3427,#3428,#1582,.T.);
#4148=EDGE_CURVE('',#3428,#3429,#1583,.T.);
#4149=EDGE_CURVE('',#3429,#3430,#1584,.T.);
#4150=EDGE_CURVE('',#3430,#3431,#1585,.T.);
#4151=EDGE_CURVE('',#3431,#3432,#1586,.T.);
#4152=EDGE_CURVE('',#3432,#3433,#3195,.T.);
#4153=EDGE_CURVE('',#3433,#3377,#3196,.T.);
#4154=EDGE_CURVE('',#3434,#3435,#1587,.T.);
#4155=EDGE_CURVE('',#3434,#3422,#1588,.T.);
#4156=EDGE_CURVE('',#3436,#3422,#1589,.T.);
#4157=EDGE_CURVE('',#3435,#3436,#1590,.T.);
#4158=EDGE_CURVE('',#3435,#3437,#1591,.T.);
#4159=EDGE_CURVE('',#3438,#3436,#1592,.T.);
#4160=EDGE_CURVE('',#3437,#3438,#1593,.T.);
#4161=EDGE_CURVE('',#3437,#3439,#1594,.T.);
#4162=EDGE_CURVE('',#3440,#3438,#1595,.T.);
#4163=EDGE_CURVE('',#3439,#3440,#1596,.T.);
#4164=EDGE_CURVE('',#3439,#3441,#1597,.T.);
#4165=EDGE_CURVE('',#3442,#3440,#1598,.T.);
#4166=EDGE_CURVE('',#3441,#3442,#1599,.T.);
#4167=EDGE_CURVE('',#3441,#3443,#1600,.T.);
#4168=EDGE_CURVE('',#3444,#3442,#1601,.T.);
#4169=EDGE_CURVE('',#3443,#3444,#1602,.T.);
#4170=EDGE_CURVE('',#3443,#3445,#1603,.T.);
#4171=EDGE_CURVE('',#3446,#3444,#1604,.T.);
#4172=EDGE_CURVE('',#3445,#3446,#1605,.T.);
#4173=EDGE_CURVE('',#3445,#3447,#1606,.T.);
#4174=EDGE_CURVE('',#3448,#3446,#1607,.T.);
#4175=EDGE_CURVE('',#3447,#3448,#1608,.T.);
#4176=EDGE_CURVE('',#3447,#3449,#1609,.T.);
#4177=EDGE_CURVE('',#3432,#3448,#1610,.T.);
#4178=EDGE_CURVE('',#3449,#3432,#1611,.T.);
#4179=EDGE_CURVE('',#3449,#3450,#1612,.T.);
#4180=EDGE_CURVE('',#3450,#3431,#1613,.T.);
#4181=EDGE_CURVE('',#3450,#3451,#1614,.T.);
#4182=EDGE_CURVE('',#3451,#3430,#1615,.T.);
#4183=EDGE_CURVE('',#3451,#3452,#1616,.T.);
#4184=EDGE_CURVE('',#3452,#3429,#1617,.T.);
#4185=EDGE_CURVE('',#3452,#3453,#1618,.T.);
#4186=EDGE_CURVE('',#3453,#3428,#1619,.T.);
#4187=EDGE_CURVE('',#3453,#3454,#1620,.T.);
#4188=EDGE_CURVE('',#3454,#3427,#1621,.T.);
#4189=EDGE_CURVE('',#3454,#3455,#1622,.T.);
#4190=EDGE_CURVE('',#3455,#3426,#1623,.T.);
#4191=EDGE_CURVE('',#3455,#3456,#1624,.T.);
#4192=EDGE_CURVE('',#3456,#3425,#1625,.T.);
#4193=EDGE_CURVE('',#3456,#3457,#1626,.T.);
#4194=EDGE_CURVE('',#3457,#3424,#1627,.T.);
#4195=EDGE_CURVE('',#3457,#3458,#1628,.T.);
#4196=EDGE_CURVE('',#3458,#3423,#1629,.T.);
#4197=EDGE_CURVE('',#3458,#3434,#1630,.T.);
#4198=EDGE_CURVE('',#3422,#3436,#3197,.T.);
#4199=EDGE_CURVE('',#3436,#3438,#3198,.T.);
#4200=EDGE_CURVE('',#3438,#3440,#3199,.T.);
#4201=EDGE_CURVE('',#3440,#3442,#3200,.T.);
#4202=EDGE_CURVE('',#3442,#3444,#3201,.T.);
#4203=EDGE_CURVE('',#3444,#3446,#3202,.T.);
#4204=EDGE_CURVE('',#3446,#3448,#3203,.T.);
#4205=EDGE_CURVE('',#3448,#3432,#3204,.T.);
#4206=EDGE_CURVE('',#3459,#3460,#1631,.T.);
#4207=EDGE_CURVE('',#3459,#3411,#1632,.T.);
#4208=EDGE_CURVE('',#3461,#3411,#1633,.T.);
#4209=EDGE_CURVE('',#3460,#3461,#1634,.T.);
#4210=EDGE_CURVE('',#3460,#3462,#1635,.T.);
#4211=EDGE_CURVE('',#3463,#3461,#1636,.T.);
#4212=EDGE_CURVE('',#3462,#3463,#1637,.T.);
#4213=EDGE_CURVE('',#3462,#3464,#1638,.T.);
#4214=EDGE_CURVE('',#3465,#3463,#1639,.T.);
#4215=EDGE_CURVE('',#3464,#3465,#1640,.T.);
#4216=EDGE_CURVE('',#3464,#3466,#1641,.T.);
#4217=EDGE_CURVE('',#3467,#3465,#1642,.T.);
#4218=EDGE_CURVE('',#3466,#3467,#1643,.T.);
#4219=EDGE_CURVE('',#3466,#3468,#1644,.T.);
#4220=EDGE_CURVE('',#3469,#3467,#1645,.T.);
#4221=EDGE_CURVE('',#3468,#3469,#1646,.T.);
#4222=EDGE_CURVE('',#3468,#3470,#1647,.T.);
#4223=EDGE_CURVE('',#3471,#3469,#1648,.T.);
#4224=EDGE_CURVE('',#3470,#3471,#1649,.T.);
#4225=EDGE_CURVE('',#3470,#3472,#1650,.T.);
#4226=EDGE_CURVE('',#3473,#3471,#1651,.T.);
#4227=EDGE_CURVE('',#3472,#3473,#1652,.T.);
#4228=EDGE_CURVE('',#3472,#3474,#1653,.T.);
#4229=EDGE_CURVE('',#3421,#3473,#1654,.T.);
#4230=EDGE_CURVE('',#3474,#3421,#1655,.T.);
#4231=EDGE_CURVE('',#3474,#3475,#1656,.T.);
#4232=EDGE_CURVE('',#3475,#3420,#1657,.T.);
#4233=EDGE_CURVE('',#3475,#3476,#1658,.T.);
#4234=EDGE_CURVE('',#3476,#3419,#1659,.T.);
#4235=EDGE_CURVE('',#3476,#3477,#1660,.T.);
#4236=EDGE_CURVE('',#3477,#3418,#1661,.T.);
#4237=EDGE_CURVE('',#3477,#3478,#1662,.T.);
#4238=EDGE_CURVE('',#3478,#3417,#1663,.T.);
#4239=EDGE_CURVE('',#3478,#3479,#1664,.T.);
#4240=EDGE_CURVE('',#3479,#3416,#1665,.T.);
#4241=EDGE_CURVE('',#3479,#3480,#1666,.T.);
#4242=EDGE_CURVE('',#3480,#3415,#1667,.T.);
#4243=EDGE_CURVE('',#3480,#3481,#1668,.T.);
#4244=EDGE_CURVE('',#3481,#3414,#1669,.T.);
#4245=EDGE_CURVE('',#3481,#3482,#1670,.T.);
#4246=EDGE_CURVE('',#3482,#3413,#1671,.T.);
#4247=EDGE_CURVE('',#3482,#3483,#1672,.T.);
#4248=EDGE_CURVE('',#3483,#3412,#1673,.T.);
#4249=EDGE_CURVE('',#3483,#3459,#1674,.T.);
#4250=EDGE_CURVE('',#3411,#3461,#3205,.T.);
#4251=EDGE_CURVE('',#3461,#3463,#3206,.T.);
#4252=EDGE_CURVE('',#3463,#3465,#3207,.T.);
#4253=EDGE_CURVE('',#3465,#3467,#3208,.T.);
#4254=EDGE_CURVE('',#3467,#3469,#3209,.T.);
#4255=EDGE_CURVE('',#3469,#3471,#3210,.T.);
#4256=EDGE_CURVE('',#3471,#3473,#3211,.T.);
#4257=EDGE_CURVE('',#3473,#3421,#3212,.T.);
#4258=EDGE_CURVE('',#3484,#3484,#3213,.T.);
#4259=EDGE_CURVE('',#3484,#3433,#1675,.T.);
#4260=EDGE_CURVE('',#3485,#3486,#100,.T.);
#4261=EDGE_CURVE('',#3486,#3485,#101,.T.);
#4262=EDGE_CURVE('',#3486,#3487,#1676,.T.);
#4263=EDGE_CURVE('',#3488,#3487,#102,.T.);
#4264=EDGE_CURVE('',#3487,#3488,#103,.T.);
#4265=EDGE_CURVE('',#3489,#3489,#3214,.T.);
#4266=EDGE_CURVE('',#3489,#3490,#1677,.T.);
#4267=EDGE_CURVE('',#3490,#3490,#3215,.T.);
#4268=EDGE_CURVE('',#3491,#3492,#1678,.T.);
#4269=EDGE_CURVE('',#3492,#3493,#1679,.T.);
#4270=EDGE_CURVE('',#3494,#3493,#1680,.T.);
#4271=EDGE_CURVE('',#3491,#3494,#1681,.T.);
#4272=EDGE_CURVE('',#3495,#3491,#1682,.T.);
#4273=EDGE_CURVE('',#3496,#3494,#1683,.T.);
#4274=EDGE_CURVE('',#3495,#3496,#1684,.T.);
#4275=EDGE_CURVE('',#3497,#3495,#1685,.T.);
#4276=EDGE_CURVE('',#3498,#3496,#1686,.T.);
#4277=EDGE_CURVE('',#3497,#3498,#1687,.T.);
#4278=EDGE_CURVE('',#3499,#3497,#1688,.T.);
#4279=EDGE_CURVE('',#3500,#3498,#1689,.T.);
#4280=EDGE_CURVE('',#3499,#3500,#1690,.T.);
#4281=EDGE_CURVE('',#3501,#3499,#1691,.T.);
#4282=EDGE_CURVE('',#3502,#3500,#1692,.T.);
#4283=EDGE_CURVE('',#3501,#3502,#1693,.T.);
#4284=EDGE_CURVE('',#3503,#3501,#1694,.T.);
#4285=EDGE_CURVE('',#3504,#3502,#1695,.T.);
#4286=EDGE_CURVE('',#3503,#3504,#1696,.T.);
#4287=EDGE_CURVE('',#3505,#3503,#1697,.T.);
#4288=EDGE_CURVE('',#3506,#3504,#1698,.T.);
#4289=EDGE_CURVE('',#3505,#3506,#1699,.T.);
#4290=EDGE_CURVE('',#3507,#3505,#1700,.T.);
#4291=EDGE_CURVE('',#3508,#3506,#1701,.T.);
#4292=EDGE_CURVE('',#3507,#3508,#1702,.T.);
#4293=EDGE_CURVE('',#3509,#3507,#1703,.T.);
#4294=EDGE_CURVE('',#3510,#3508,#1704,.T.);
#4295=EDGE_CURVE('',#3509,#3510,#1705,.T.);
#4296=EDGE_CURVE('',#3511,#3509,#1706,.T.);
#4297=EDGE_CURVE('',#3512,#3510,#1707,.T.);
#4298=EDGE_CURVE('',#3511,#3512,#1708,.T.);
#4299=EDGE_CURVE('',#3513,#3511,#1709,.T.);
#4300=EDGE_CURVE('',#3514,#3512,#1710,.T.);
#4301=EDGE_CURVE('',#3513,#3514,#1711,.T.);
#4302=EDGE_CURVE('',#3515,#3513,#1712,.T.);
#4303=EDGE_CURVE('',#3516,#3514,#1713,.T.);
#4304=EDGE_CURVE('',#3515,#3516,#1714,.T.);
#4305=EDGE_CURVE('',#3517,#3515,#1715,.T.);
#4306=EDGE_CURVE('',#3518,#3516,#1716,.T.);
#4307=EDGE_CURVE('',#3517,#3518,#1717,.T.);
#4308=EDGE_CURVE('',#3519,#3517,#1718,.T.);
#4309=EDGE_CURVE('',#3520,#3518,#1719,.T.);
#4310=EDGE_CURVE('',#3519,#3520,#1720,.T.);
#4311=EDGE_CURVE('',#3521,#3519,#1721,.T.);
#4312=EDGE_CURVE('',#3522,#3520,#1722,.T.);
#4313=EDGE_CURVE('',#3521,#3522,#1723,.T.);
#4314=EDGE_CURVE('',#3523,#3521,#1724,.T.);
#4315=EDGE_CURVE('',#3524,#3522,#1725,.T.);
#4316=EDGE_CURVE('',#3523,#3524,#1726,.T.);
#4317=EDGE_CURVE('',#3525,#3523,#1727,.T.);
#4318=EDGE_CURVE('',#3526,#3524,#1728,.T.);
#4319=EDGE_CURVE('',#3525,#3526,#1729,.T.);
#4320=EDGE_CURVE('',#3492,#3525,#1730,.T.);
#4321=EDGE_CURVE('',#3493,#3526,#1731,.T.);
#4322=EDGE_CURVE('',#3526,#3524,#3216,.T.);
#4323=EDGE_CURVE('',#3524,#3522,#3217,.T.);
#4324=EDGE_CURVE('',#3522,#3520,#3218,.T.);
#4325=EDGE_CURVE('',#3520,#3518,#3219,.T.);
#4326=EDGE_CURVE('',#3518,#3516,#3220,.T.);
#4327=EDGE_CURVE('',#3516,#3514,#3221,.T.);
#4328=EDGE_CURVE('',#3527,#3526,#3222,.T.);
#4329=EDGE_CURVE('',#3528,#3527,#3223,.T.);
#4330=EDGE_CURVE('',#3528,#3529,#1732,.T.);
#4331=EDGE_CURVE('',#3529,#3530,#1733,.T.);
#4332=EDGE_CURVE('',#3530,#3531,#1734,.T.);
#4333=EDGE_CURVE('',#3531,#3532,#1735,.T.);
#4334=EDGE_CURVE('',#3532,#3533,#1736,.T.);
#4335=EDGE_CURVE('',#3533,#3534,#1737,.T.);
#4336=EDGE_CURVE('',#3534,#3535,#1738,.T.);
#4337=EDGE_CURVE('',#3535,#3536,#1739,.T.);
#4338=EDGE_CURVE('',#3536,#3537,#1740,.T.);
#4339=EDGE_CURVE('',#3537,#3538,#1741,.T.);
#4340=EDGE_CURVE('',#3539,#3538,#3224,.T.);
#4341=EDGE_CURVE('',#3539,#3540,#1742,.T.);
#4342=EDGE_CURVE('',#3540,#3541,#1743,.T.);
#4343=EDGE_CURVE('',#3541,#3542,#1744,.T.);
#4344=EDGE_CURVE('',#3542,#3543,#1745,.T.);
#4345=EDGE_CURVE('',#3543,#3544,#1746,.T.);
#4346=EDGE_CURVE('',#3544,#3545,#1747,.T.);
#4347=EDGE_CURVE('',#3545,#3546,#1748,.T.);
#4348=EDGE_CURVE('',#3546,#3547,#1749,.T.);
#4349=EDGE_CURVE('',#3547,#3548,#1750,.T.);
#4350=EDGE_CURVE('',#3548,#3549,#1751,.T.);
#4351=EDGE_CURVE('',#3510,#3549,#3225,.T.);
#4352=EDGE_CURVE('',#3512,#3510,#3226,.T.);
#4353=EDGE_CURVE('',#3514,#3512,#3227,.T.);
#4354=EDGE_CURVE('',#3550,#3551,#1752,.T.);
#4355=EDGE_CURVE('',#3551,#3537,#1753,.T.);
#4356=EDGE_CURVE('',#3550,#3536,#1754,.T.);
#4357=EDGE_CURVE('',#3552,#3550,#1755,.T.);
#4358=EDGE_CURVE('',#3552,#3535,#1756,.T.);
#4359=EDGE_CURVE('',#3553,#3552,#1757,.T.);
#4360=EDGE_CURVE('',#3553,#3534,#1758,.T.);
#4361=EDGE_CURVE('',#3554,#3553,#1759,.T.);
#4362=EDGE_CURVE('',#3554,#3533,#1760,.T.);
#4363=EDGE_CURVE('',#3555,#3554,#1761,.T.);
#4364=EDGE_CURVE('',#3555,#3532,#1762,.T.);
#4365=EDGE_CURVE('',#3556,#3555,#1763,.T.);
#4366=EDGE_CURVE('',#3556,#3531,#1764,.T.);
#4367=EDGE_CURVE('',#3557,#3556,#1765,.T.);
#4368=EDGE_CURVE('',#3557,#3530,#1766,.T.);
#4369=EDGE_CURVE('',#3558,#3557,#1767,.T.);
#4370=EDGE_CURVE('',#3558,#3529,#1768,.T.);
#4371=EDGE_CURVE('',#3559,#3558,#1769,.T.);
#4372=EDGE_CURVE('',#3559,#3528,#1770,.T.);
#4373=EDGE_CURVE('',#3560,#3559,#1771,.T.);
#4374=EDGE_CURVE('',#3561,#3528,#1772,.T.);
#4375=EDGE_CURVE('',#3560,#3561,#1773,.T.);
#4376=EDGE_CURVE('',#3562,#3560,#1774,.T.);
#4377=EDGE_CURVE('',#3563,#3561,#1775,.T.);
#4378=EDGE_CURVE('',#3562,#3563,#1776,.T.);
#4379=EDGE_CURVE('',#3564,#3562,#1777,.T.);
#4380=EDGE_CURVE('',#3565,#3563,#1778,.T.);
#4381=EDGE_CURVE('',#3564,#3565,#1779,.T.);
#4382=EDGE_CURVE('',#3566,#3564,#1780,.T.);
#4383=EDGE_CURVE('',#3567,#3565,#1781,.T.);
#4384=EDGE_CURVE('',#3566,#3567,#1782,.T.);
#4385=EDGE_CURVE('',#3568,#3566,#1783,.T.);
#4386=EDGE_CURVE('',#3569,#3567,#1784,.T.);
#4387=EDGE_CURVE('',#3568,#3569,#1785,.T.);
#4388=EDGE_CURVE('',#3570,#3568,#1786,.T.);
#4389=EDGE_CURVE('',#3571,#3569,#1787,.T.);
#4390=EDGE_CURVE('',#3570,#3571,#1788,.T.);
#4391=EDGE_CURVE('',#3572,#3570,#1789,.T.);
#4392=EDGE_CURVE('',#3573,#3571,#1790,.T.);
#4393=EDGE_CURVE('',#3572,#3573,#1791,.T.);
#4394=EDGE_CURVE('',#3574,#3572,#1792,.T.);
#4395=EDGE_CURVE('',#3538,#3573,#1793,.T.);
#4396=EDGE_CURVE('',#3574,#3538,#1794,.T.);
#4397=EDGE_CURVE('',#3551,#3574,#1795,.T.);
#4398=EDGE_CURVE('',#3538,#3573,#3228,.T.);
#4399=EDGE_CURVE('',#3573,#3571,#3229,.T.);
#4400=EDGE_CURVE('',#3571,#3569,#3230,.T.);
#4401=EDGE_CURVE('',#3569,#3567,#3231,.T.);
#4402=EDGE_CURVE('',#3567,#3565,#3232,.T.);
#4403=EDGE_CURVE('',#3565,#3563,#3233,.T.);
#4404=EDGE_CURVE('',#3561,#3528,#3234,.T.);
#4405=EDGE_CURVE('',#3563,#3561,#3235,.T.);
#4406=EDGE_CURVE('',#3575,#3576,#1796,.T.);
#4407=EDGE_CURVE('',#3576,#3548,#1797,.T.);
#4408=EDGE_CURVE('',#3575,#3547,#1798,.T.);
#4409=EDGE_CURVE('',#3577,#3575,#1799,.T.);
#4410=EDGE_CURVE('',#3577,#3546,#1800,.T.);
#4411=EDGE_CURVE('',#3578,#3577,#1801,.T.);
#4412=EDGE_CURVE('',#3578,#3545,#1802,.T.);
#4413=EDGE_CURVE('',#3579,#3578,#1803,.T.);
#4414=EDGE_CURVE('',#3579,#3544,#1804,.T.);
#4415=EDGE_CURVE('',#3580,#3579,#1805,.T.);
#4416=EDGE_CURVE('',#3580,#3543,#1806,.T.);
#4417=EDGE_CURVE('',#3581,#3580,#1807,.T.);
#4418=EDGE_CURVE('',#3581,#3542,#1808,.T.);
#4419=EDGE_CURVE('',#3582,#3581,#1809,.T.);
#4420=EDGE_CURVE('',#3582,#3541,#1810,.T.);
#4421=EDGE_CURVE('',#3583,#3582,#1811,.T.);
#4422=EDGE_CURVE('',#3583,#3540,#1812,.T.);
#4423=EDGE_CURVE('',#3584,#3583,#1813,.T.);
#4424=EDGE_CURVE('',#3584,#3539,#1814,.T.);
#4425=EDGE_CURVE('',#3585,#3584,#1815,.T.);
#4426=EDGE_CURVE('',#3586,#3539,#1816,.T.);
#4427=EDGE_CURVE('',#3585,#3586,#1817,.T.);
#4428=EDGE_CURVE('',#3587,#3585,#1818,.T.);
#4429=EDGE_CURVE('',#3588,#3586,#1819,.T.);
#4430=EDGE_CURVE('',#3587,#3588,#1820,.T.);
#4431=EDGE_CURVE('',#3589,#3587,#1821,.T.);
#4432=EDGE_CURVE('',#3590,#3588,#1822,.T.);
#4433=EDGE_CURVE('',#3589,#3590,#1823,.T.);
#4434=EDGE_CURVE('',#3591,#3589,#1824,.T.);
#4435=EDGE_CURVE('',#3592,#3590,#1825,.T.);
#4436=EDGE_CURVE('',#3591,#3592,#1826,.T.);
#4437=EDGE_CURVE('',#3593,#3591,#1827,.T.);
#4438=EDGE_CURVE('',#3594,#3592,#1828,.T.);
#4439=EDGE_CURVE('',#3593,#3594,#1829,.T.);
#4440=EDGE_CURVE('',#3595,#3593,#1830,.T.);
#4441=EDGE_CURVE('',#3596,#3594,#1831,.T.);
#4442=EDGE_CURVE('',#3595,#3596,#1832,.T.);
#4443=EDGE_CURVE('',#3597,#3595,#1833,.T.);
#4444=EDGE_CURVE('',#3598,#3596,#1834,.T.);
#4445=EDGE_CURVE('',#3597,#3598,#1835,.T.);
#4446=EDGE_CURVE('',#3599,#3597,#1836,.T.);
#4447=EDGE_CURVE('',#3549,#3598,#1837,.T.);
#4448=EDGE_CURVE('',#3599,#3549,#1838,.T.);
#4449=EDGE_CURVE('',#3576,#3599,#1839,.T.);
#4450=EDGE_CURVE('',#3549,#3598,#3236,.T.);
#4451=EDGE_CURVE('',#3598,#3596,#3237,.T.);
#4452=EDGE_CURVE('',#3596,#3594,#3238,.T.);
#4453=EDGE_CURVE('',#3594,#3592,#3239,.T.);
#4454=EDGE_CURVE('',#3592,#3590,#3240,.T.);
#4455=EDGE_CURVE('',#3590,#3588,#3241,.T.);
#4456=EDGE_CURVE('',#3586,#3539,#3242,.T.);
#4457=EDGE_CURVE('',#3588,#3586,#3243,.T.);
#4458=EDGE_CURVE('',#3600,#3600,#3244,.T.);
#4459=EDGE_CURVE('',#3600,#3527,#1840,.T.);
#4460=EDGE_CURVE('',#3601,#3602,#1841,.T.);
#4461=EDGE_CURVE('',#3603,#3601,#1842,.T.);
#4462=EDGE_CURVE('',#3604,#3603,#1843,.T.);
#4463=EDGE_CURVE('',#3605,#3604,#1844,.T.);
#4464=EDGE_CURVE('',#3606,#3605,#1845,.T.);
#4465=EDGE_CURVE('',#3607,#3606,#1846,.T.);
#4466=EDGE_CURVE('',#3608,#3607,#1847,.T.);
#4467=EDGE_CURVE('',#3609,#3608,#1848,.T.);
#4468=EDGE_CURVE('',#3609,#3610,#3245,.T.);
#4469=EDGE_CURVE('',#3611,#3610,#1849,.T.);
#4470=EDGE_CURVE('',#3612,#3611,#1850,.T.);
#4471=EDGE_CURVE('',#3613,#3612,#1851,.T.);
#4472=EDGE_CURVE('',#3614,#3613,#1852,.T.);
#4473=EDGE_CURVE('',#3615,#3614,#1853,.T.);
#4474=EDGE_CURVE('',#3616,#3615,#1854,.T.);
#4475=EDGE_CURVE('',#3617,#3616,#1855,.T.);
#4476=EDGE_CURVE('',#3618,#3617,#1856,.T.);
#4477=EDGE_CURVE('',#3618,#3619,#3246,.T.);
#4478=EDGE_CURVE('',#3620,#3619,#1857,.T.);
#4479=EDGE_CURVE('',#3621,#3620,#1858,.T.);
#4480=EDGE_CURVE('',#3622,#3621,#1859,.T.);
#4481=EDGE_CURVE('',#3623,#3622,#1860,.T.);
#4482=EDGE_CURVE('',#3624,#3623,#1861,.T.);
#4483=EDGE_CURVE('',#3625,#3624,#1862,.T.);
#4484=EDGE_CURVE('',#3626,#3625,#1863,.T.);
#4485=EDGE_CURVE('',#3627,#3626,#1864,.T.);
#4486=EDGE_CURVE('',#3627,#3628,#3247,.T.);
#4487=EDGE_CURVE('',#3629,#3628,#1865,.T.);
#4488=EDGE_CURVE('',#3630,#3629,#1866,.T.);
#4489=EDGE_CURVE('',#3631,#3630,#1867,.T.);
#4490=EDGE_CURVE('',#3632,#3631,#1868,.T.);
#4491=EDGE_CURVE('',#3633,#3632,#1869,.T.);
#4492=EDGE_CURVE('',#3634,#3633,#1870,.T.);
#4493=EDGE_CURVE('',#3635,#3634,#1871,.T.);
#4494=EDGE_CURVE('',#3636,#3635,#1872,.T.);
#4495=EDGE_CURVE('',#3636,#3637,#3248,.T.);
#4496=EDGE_CURVE('',#3638,#3637,#1873,.T.);
#4497=EDGE_CURVE('',#3639,#3638,#1874,.T.);
#4498=EDGE_CURVE('',#3640,#3639,#1875,.T.);
#4499=EDGE_CURVE('',#3641,#3640,#1876,.T.);
#4500=EDGE_CURVE('',#3642,#3641,#1877,.T.);
#4501=EDGE_CURVE('',#3643,#3642,#1878,.T.);
#4502=EDGE_CURVE('',#3644,#3643,#1879,.T.);
#4503=EDGE_CURVE('',#3645,#3644,#1880,.T.);
#4504=EDGE_CURVE('',#3645,#3646,#3249,.T.);
#4505=EDGE_CURVE('',#3647,#3646,#1881,.T.);
#4506=EDGE_CURVE('',#3648,#3647,#1882,.T.);
#4507=EDGE_CURVE('',#3649,#3648,#1883,.T.);
#4508=EDGE_CURVE('',#3650,#3649,#1884,.T.);
#4509=EDGE_CURVE('',#3651,#3650,#1885,.T.);
#4510=EDGE_CURVE('',#3652,#3651,#1886,.T.);
#4511=EDGE_CURVE('',#3653,#3652,#1887,.T.);
#4512=EDGE_CURVE('',#3654,#3653,#1888,.T.);
#4513=EDGE_CURVE('',#3654,#3602,#3250,.T.);
#4514=EDGE_CURVE('',#3655,#3645,#1889,.T.);
#4515=EDGE_CURVE('',#3656,#3655,#3251,.T.);
#4516=EDGE_CURVE('',#3646,#3656,#1890,.T.);
#4517=EDGE_CURVE('',#3657,#3609,#1891,.T.);
#4518=EDGE_CURVE('',#3658,#3657,#3252,.T.);
#4519=EDGE_CURVE('',#3610,#3658,#1892,.T.);
#4520=EDGE_CURVE('',#3659,#3627,#1893,.T.);
#4521=EDGE_CURVE('',#3660,#3659,#3253,.T.);
#4522=EDGE_CURVE('',#3628,#3660,#1894,.T.);
#4523=EDGE_CURVE('',#3637,#3661,#1895,.T.);
#4524=EDGE_CURVE('',#3662,#3636,#1896,.T.);
#4525=EDGE_CURVE('',#3661,#3662,#3254,.T.);
#4526=EDGE_CURVE('',#3619,#3663,#1897,.T.);
#4527=EDGE_CURVE('',#3664,#3618,#1898,.T.);
#4528=EDGE_CURVE('',#3663,#3664,#3255,.T.);
#4529=EDGE_CURVE('',#3602,#3665,#1899,.T.);
#4530=EDGE_CURVE('',#3666,#3654,#1900,.T.);
#4531=EDGE_CURVE('',#3665,#3666,#3256,.T.);
#4532=EDGE_CURVE('',#3665,#3667,#1901,.T.);
#4533=EDGE_CURVE('',#3668,#3666,#1902,.T.);
#4534=EDGE_CURVE('',#3669,#3668,#1903,.T.);
#4535=EDGE_CURVE('',#3670,#3669,#1904,.T.);
#4536=EDGE_CURVE('',#3671,#3670,#1905,.T.);
#4537=EDGE_CURVE('',#3672,#3671,#1906,.T.);
#4538=EDGE_CURVE('',#3673,#3672,#1907,.T.);
#4539=EDGE_CURVE('',#3674,#3673,#1908,.T.);
#4540=EDGE_CURVE('',#3656,#3674,#1909,.T.);
#4541=EDGE_CURVE('',#3675,#3655,#1910,.T.);
#4542=EDGE_CURVE('',#3676,#3675,#1911,.T.);
#4543=EDGE_CURVE('',#3677,#3676,#1912,.T.);
#4544=EDGE_CURVE('',#3678,#3677,#1913,.T.);
#4545=EDGE_CURVE('',#3679,#3678,#1914,.T.);
#4546=EDGE_CURVE('',#3680,#3679,#1915,.T.);
#4547=EDGE_CURVE('',#3681,#3680,#1916,.T.);
#4548=EDGE_CURVE('',#3661,#3681,#1917,.T.);
#4549=EDGE_CURVE('',#3682,#3662,#1918,.T.);
#4550=EDGE_CURVE('',#3683,#3682,#1919,.T.);
#4551=EDGE_CURVE('',#3684,#3683,#1920,.T.);
#4552=EDGE_CURVE('',#3685,#3684,#1921,.T.);
#4553=EDGE_CURVE('',#3686,#3685,#1922,.T.);
#4554=EDGE_CURVE('',#3687,#3686,#1923,.T.);
#4555=EDGE_CURVE('',#3688,#3687,#1924,.T.);
#4556=EDGE_CURVE('',#3660,#3688,#1925,.T.);
#4557=EDGE_CURVE('',#3689,#3659,#1926,.T.);
#4558=EDGE_CURVE('',#3690,#3689,#1927,.T.);
#4559=EDGE_CURVE('',#3691,#3690,#1928,.T.);
#4560=EDGE_CURVE('',#3692,#3691,#1929,.T.);
#4561=EDGE_CURVE('',#3693,#3692,#1930,.T.);
#4562=EDGE_CURVE('',#3694,#3693,#1931,.T.);
#4563=EDGE_CURVE('',#3695,#3694,#1932,.T.);
#4564=EDGE_CURVE('',#3663,#3695,#1933,.T.);
#4565=EDGE_CURVE('',#3696,#3664,#1934,.T.);
#4566=EDGE_CURVE('',#3697,#3696,#1935,.T.);
#4567=EDGE_CURVE('',#3698,#3697,#1936,.T.);
#4568=EDGE_CURVE('',#3699,#3698,#1937,.T.);
#4569=EDGE_CURVE('',#3700,#3699,#1938,.T.);
#4570=EDGE_CURVE('',#3701,#3700,#1939,.T.);
#4571=EDGE_CURVE('',#3702,#3701,#1940,.T.);
#4572=EDGE_CURVE('',#3658,#3702,#1941,.T.);
#4573=EDGE_CURVE('',#3703,#3657,#1942,.T.);
#4574=EDGE_CURVE('',#3704,#3703,#1943,.T.);
#4575=EDGE_CURVE('',#3705,#3704,#1944,.T.);
#4576=EDGE_CURVE('',#3706,#3705,#1945,.T.);
#4577=EDGE_CURVE('',#3707,#3706,#1946,.T.);
#4578=EDGE_CURVE('',#3708,#3707,#1947,.T.);
#4579=EDGE_CURVE('',#3667,#3708,#1948,.T.);
#4580=EDGE_CURVE('',#3674,#3709,#1949,.T.);
#4581=EDGE_CURVE('',#3710,#3709,#1950,.T.);
#4582=EDGE_CURVE('',#3711,#3710,#1951,.T.);
#4583=EDGE_CURVE('',#3712,#3711,#1952,.T.);
#4584=EDGE_CURVE('',#3712,#3647,#1953,.T.);
#4585=EDGE_CURVE('',#3673,#3713,#1954,.T.);
#4586=EDGE_CURVE('',#3709,#3713,#1955,.T.);
#4587=EDGE_CURVE('',#3714,#3712,#1956,.T.);
#4588=EDGE_CURVE('',#3714,#3648,#1957,.T.);
#4589=EDGE_CURVE('',#3672,#3715,#1958,.T.);
#4590=EDGE_CURVE('',#3713,#3715,#1959,.T.);
#4591=EDGE_CURVE('',#3671,#3716,#1960,.T.);
#4592=EDGE_CURVE('',#3715,#3716,#1961,.T.);
#4593=EDGE_CURVE('',#3670,#3717,#1962,.T.);
#4594=EDGE_CURVE('',#3716,#3717,#1963,.T.);
#4595=EDGE_CURVE('',#3669,#3718,#1964,.T.);
#4596=EDGE_CURVE('',#3717,#3718,#1965,.T.);
#4597=EDGE_CURVE('',#3719,#3668,#1966,.T.);
#4598=EDGE_CURVE('',#3718,#3719,#1967,.T.);
#4599=EDGE_CURVE('',#3720,#3721,#1968,.T.);
#4600=EDGE_CURVE('',#3721,#3722,#1969,.T.);
#4601=EDGE_CURVE('',#3722,#3723,#1970,.T.);
#4602=EDGE_CURVE('',#3723,#3724,#1971,.T.);
#4603=EDGE_CURVE('',#3724,#3725,#1972,.T.);
#4604=EDGE_CURVE('',#3725,#3714,#1973,.T.);
#4605=EDGE_CURVE('',#3711,#3726,#1974,.T.);
#4606=EDGE_CURVE('',#3726,#3727,#1975,.T.);
#4607=EDGE_CURVE('',#3727,#3728,#1976,.T.);
#4608=EDGE_CURVE('',#3728,#3729,#1977,.T.);
#4609=EDGE_CURVE('',#3729,#3730,#1978,.T.);
#4610=EDGE_CURVE('',#3730,#3720,#1979,.T.);
#4611=EDGE_CURVE('',#3722,#3652,#1980,.T.);
#4612=EDGE_CURVE('',#3653,#3721,#1981,.T.);
#4613=EDGE_CURVE('',#3723,#3651,#1982,.T.);
#4614=EDGE_CURVE('',#3724,#3650,#1983,.T.);
#4615=EDGE_CURVE('',#3725,#3649,#1984,.T.);
#4616=EDGE_CURVE('',#3731,#3710,#1985,.T.);
#4617=EDGE_CURVE('',#3726,#3731,#1986,.T.);
#4618=EDGE_CURVE('',#3732,#3731,#1987,.T.);
#4619=EDGE_CURVE('',#3727,#3732,#1988,.T.);
#4620=EDGE_CURVE('',#3733,#3732,#1989,.T.);
#4621=EDGE_CURVE('',#3728,#3733,#1990,.T.);
#4622=EDGE_CURVE('',#3734,#3733,#1991,.T.);
#4623=EDGE_CURVE('',#3729,#3734,#1992,.T.);
#4624=EDGE_CURVE('',#3735,#3734,#1993,.T.);
#4625=EDGE_CURVE('',#3730,#3735,#1994,.T.);
#4626=EDGE_CURVE('',#3736,#3735,#1995,.T.);
#4627=EDGE_CURVE('',#3720,#3736,#1996,.T.);
#4628=EDGE_CURVE('',#3719,#3736,#1997,.T.);
#4629=EDGE_CURVE('',#3702,#3737,#1998,.T.);
#4630=EDGE_CURVE('',#3738,#3737,#1999,.T.);
#4631=EDGE_CURVE('',#3739,#3738,#2000,.T.);
#4632=EDGE_CURVE('',#3740,#3739,#2001,.T.);
#4633=EDGE_CURVE('',#3740,#3611,#2002,.T.);
#4634=EDGE_CURVE('',#3701,#3741,#2003,.T.);
#4635=EDGE_CURVE('',#3737,#3741,#2004,.T.);
#4636=EDGE_CURVE('',#3742,#3740,#2005,.T.);
#4637=EDGE_CURVE('',#3742,#3612,#2006,.T.);
#4638=EDGE_CURVE('',#3700,#3743,#2007,.T.);
#4639=EDGE_CURVE('',#3741,#3743,#2008,.T.);
#4640=EDGE_CURVE('',#3699,#3744,#2009,.T.);
#4641=EDGE_CURVE('',#3743,#3744,#2010,.T.);
#4642=EDGE_CURVE('',#3698,#3745,#2011,.T.);
#4643=EDGE_CURVE('',#3744,#3745,#2012,.T.);
#4644=EDGE_CURVE('',#3697,#3746,#2013,.T.);
#4645=EDGE_CURVE('',#3745,#3746,#2014,.T.);
#4646=EDGE_CURVE('',#3747,#3696,#2015,.T.);
#4647=EDGE_CURVE('',#3746,#3747,#2016,.T.);
#4648=EDGE_CURVE('',#3748,#3749,#2017,.T.);
#4649=EDGE_CURVE('',#3749,#3750,#2018,.T.);
#4650=EDGE_CURVE('',#3750,#3751,#2019,.T.);
#4651=EDGE_CURVE('',#3751,#3752,#2020,.T.);
#4652=EDGE_CURVE('',#3752,#3753,#2021,.T.);
#4653=EDGE_CURVE('',#3753,#3742,#2022,.T.);
#4654=EDGE_CURVE('',#3739,#3754,#2023,.T.);
#4655=EDGE_CURVE('',#3754,#3755,#2024,.T.);
#4656=EDGE_CURVE('',#3755,#3756,#2025,.T.);
#4657=EDGE_CURVE('',#3756,#3757,#2026,.T.);
#4658=EDGE_CURVE('',#3757,#3758,#2027,.T.);
#4659=EDGE_CURVE('',#3758,#3748,#2028,.T.);
#4660=EDGE_CURVE('',#3750,#3616,#2029,.T.);
#4661=EDGE_CURVE('',#3617,#3749,#2030,.T.);
#4662=EDGE_CURVE('',#3751,#3615,#2031,.T.);
#4663=EDGE_CURVE('',#3752,#3614,#2032,.T.);
#4664=EDGE_CURVE('',#3753,#3613,#2033,.T.);
#4665=EDGE_CURVE('',#3759,#3738,#2034,.T.);
#4666=EDGE_CURVE('',#3754,#3759,#2035,.T.);
#4667=EDGE_CURVE('',#3760,#3759,#2036,.T.);
#4668=EDGE_CURVE('',#3755,#3760,#2037,.T.);
#4669=EDGE_CURVE('',#3761,#3760,#2038,.T.);
#4670=EDGE_CURVE('',#3756,#3761,#2039,.T.);
#4671=EDGE_CURVE('',#3762,#3761,#2040,.T.);
#4672=EDGE_CURVE('',#3757,#3762,#2041,.T.);
#4673=EDGE_CURVE('',#3763,#3762,#2042,.T.);
#4674=EDGE_CURVE('',#3758,#3763,#2043,.T.);
#4675=EDGE_CURVE('',#3764,#3763,#2044,.T.);
#4676=EDGE_CURVE('',#3748,#3764,#2045,.T.);
#4677=EDGE_CURVE('',#3747,#3764,#2046,.T.);
#4678=EDGE_CURVE('',#3688,#3765,#2047,.T.);
#4679=EDGE_CURVE('',#3766,#3765,#2048,.T.);
#4680=EDGE_CURVE('',#3767,#3766,#2049,.T.);
#4681=EDGE_CURVE('',#3768,#3767,#2050,.T.);
#4682=EDGE_CURVE('',#3768,#3629,#2051,.T.);
#4683=EDGE_CURVE('',#3687,#3769,#2052,.T.);
#4684=EDGE_CURVE('',#3765,#3769,#2053,.T.);
#4685=EDGE_CURVE('',#3770,#3768,#2054,.T.);
#4686=EDGE_CURVE('',#3770,#3630,#2055,.T.);
#4687=EDGE_CURVE('',#3686,#3771,#2056,.T.);
#4688=EDGE_CURVE('',#3769,#3771,#2057,.T.);
#4689=EDGE_CURVE('',#3685,#3772,#2058,.T.);
#4690=EDGE_CURVE('',#3771,#3772,#2059,.T.);
#4691=EDGE_CURVE('',#3684,#3773,#2060,.T.);
#4692=EDGE_CURVE('',#3772,#3773,#2061,.T.);
#4693=EDGE_CURVE('',#3683,#3774,#2062,.T.);
#4694=EDGE_CURVE('',#3773,#3774,#2063,.T.);
#4695=EDGE_CURVE('',#3775,#3682,#2064,.T.);
#4696=EDGE_CURVE('',#3774,#3775,#2065,.T.);
#4697=EDGE_CURVE('',#3776,#3777,#2066,.T.);
#4698=EDGE_CURVE('',#3777,#3778,#2067,.T.);
#4699=EDGE_CURVE('',#3778,#3779,#2068,.T.);
#4700=EDGE_CURVE('',#3779,#3780,#2069,.T.);
#4701=EDGE_CURVE('',#3780,#3781,#2070,.T.);
#4702=EDGE_CURVE('',#3781,#3770,#2071,.T.);
#4703=EDGE_CURVE('',#3767,#3782,#2072,.T.);
#4704=EDGE_CURVE('',#3782,#3783,#2073,.T.);
#4705=EDGE_CURVE('',#3783,#3784,#2074,.T.);
#4706=EDGE_CURVE('',#3784,#3785,#2075,.T.);
#4707=EDGE_CURVE('',#3785,#3786,#2076,.T.);
#4708=EDGE_CURVE('',#3786,#3776,#2077,.T.);
#4709=EDGE_CURVE('',#3778,#3634,#2078,.T.);
#4710=EDGE_CURVE('',#3635,#3777,#2079,.T.);
#4711=EDGE_CURVE('',#3779,#3633,#2080,.T.);
#4712=EDGE_CURVE('',#3780,#3632,#2081,.T.);
#4713=EDGE_CURVE('',#3781,#3631,#2082,.T.);
#4714=EDGE_CURVE('',#3787,#3766,#2083,.T.);
#4715=EDGE_CURVE('',#3782,#3787,#2084,.T.);
#4716=EDGE_CURVE('',#3788,#3787,#2085,.T.);
#4717=EDGE_CURVE('',#3783,#3788,#2086,.T.);
#4718=EDGE_CURVE('',#3789,#3788,#2087,.T.);
#4719=EDGE_CURVE('',#3784,#3789,#2088,.T.);
#4720=EDGE_CURVE('',#3790,#3789,#2089,.T.);
#4721=EDGE_CURVE('',#3785,#3790,#2090,.T.);
#4722=EDGE_CURVE('',#3791,#3790,#2091,.T.);
#4723=EDGE_CURVE('',#3786,#3791,#2092,.T.);
#4724=EDGE_CURVE('',#3792,#3791,#2093,.T.);
#4725=EDGE_CURVE('',#3776,#3792,#2094,.T.);
#4726=EDGE_CURVE('',#3775,#3792,#2095,.T.);
#4727=EDGE_CURVE('',#3681,#3793,#2096,.T.);
#4728=EDGE_CURVE('',#3794,#3793,#2097,.T.);
#4729=EDGE_CURVE('',#3795,#3794,#2098,.T.);
#4730=EDGE_CURVE('',#3796,#3795,#2099,.T.);
#4731=EDGE_CURVE('',#3796,#3638,#2100,.T.);
#4732=EDGE_CURVE('',#3680,#3797,#2101,.T.);
#4733=EDGE_CURVE('',#3793,#3797,#2102,.T.);
#4734=EDGE_CURVE('',#3798,#3796,#2103,.T.);
#4735=EDGE_CURVE('',#3798,#3639,#2104,.T.);
#4736=EDGE_CURVE('',#3679,#3799,#2105,.T.);
#4737=EDGE_CURVE('',#3797,#3799,#2106,.T.);
#4738=EDGE_CURVE('',#3678,#3800,#2107,.T.);
#4739=EDGE_CURVE('',#3799,#3800,#2108,.T.);
#4740=EDGE_CURVE('',#3677,#3801,#2109,.T.);
#4741=EDGE_CURVE('',#3800,#3801,#2110,.T.);
#4742=EDGE_CURVE('',#3676,#3802,#2111,.T.);
#4743=EDGE_CURVE('',#3801,#3802,#2112,.T.);
#4744=EDGE_CURVE('',#3803,#3675,#2113,.T.);
#4745=EDGE_CURVE('',#3802,#3803,#2114,.T.);
#4746=EDGE_CURVE('',#3804,#3805,#2115,.T.);
#4747=EDGE_CURVE('',#3805,#3806,#2116,.T.);
#4748=EDGE_CURVE('',#3806,#3807,#2117,.T.);
#4749=EDGE_CURVE('',#3807,#3808,#2118,.T.);
#4750=EDGE_CURVE('',#3808,#3809,#2119,.T.);
#4751=EDGE_CURVE('',#3809,#3798,#2120,.T.);
#4752=EDGE_CURVE('',#3795,#3810,#2121,.T.);
#4753=EDGE_CURVE('',#3810,#3811,#2122,.T.);
#4754=EDGE_CURVE('',#3811,#3812,#2123,.T.);
#4755=EDGE_CURVE('',#3812,#3813,#2124,.T.);
#4756=EDGE_CURVE('',#3813,#3814,#2125,.T.);
#4757=EDGE_CURVE('',#3814,#3804,#2126,.T.);
#4758=EDGE_CURVE('',#3806,#3643,#2127,.T.);
#4759=EDGE_CURVE('',#3644,#3805,#2128,.T.);
#4760=EDGE_CURVE('',#3807,#3642,#2129,.T.);
#4761=EDGE_CURVE('',#3808,#3641,#2130,.T.);
#4762=EDGE_CURVE('',#3809,#3640,#2131,.T.);
#4763=EDGE_CURVE('',#3815,#3794,#2132,.T.);
#4764=EDGE_CURVE('',#3810,#3815,#2133,.T.);
#4765=EDGE_CURVE('',#3816,#3815,#2134,.T.);
#4766=EDGE_CURVE('',#3811,#3816,#2135,.T.);
#4767=EDGE_CURVE('',#3817,#3816,#2136,.T.);
#4768=EDGE_CURVE('',#3812,#3817,#2137,.T.);
#4769=EDGE_CURVE('',#3818,#3817,#2138,.T.);
#4770=EDGE_CURVE('',#3813,#3818,#2139,.T.);
#4771=EDGE_CURVE('',#3819,#3818,#2140,.T.);
#4772=EDGE_CURVE('',#3814,#3819,#2141,.T.);
#4773=EDGE_CURVE('',#3820,#3819,#2142,.T.);
#4774=EDGE_CURVE('',#3804,#3820,#2143,.T.);
#4775=EDGE_CURVE('',#3803,#3820,#2144,.T.);
#4776=EDGE_CURVE('',#3695,#3821,#2145,.T.);
#4777=EDGE_CURVE('',#3822,#3821,#2146,.T.);
#4778=EDGE_CURVE('',#3823,#3822,#2147,.T.);
#4779=EDGE_CURVE('',#3824,#3823,#2148,.T.);
#4780=EDGE_CURVE('',#3824,#3620,#2149,.T.);
#4781=EDGE_CURVE('',#3694,#3825,#2150,.T.);
#4782=EDGE_CURVE('',#3821,#3825,#2151,.T.);
#4783=EDGE_CURVE('',#3826,#3824,#2152,.T.);
#4784=EDGE_CURVE('',#3826,#3621,#2153,.T.);
#4785=EDGE_CURVE('',#3693,#3827,#2154,.T.);
#4786=EDGE_CURVE('',#3825,#3827,#2155,.T.);
#4787=EDGE_CURVE('',#3692,#3828,#2156,.T.);
#4788=EDGE_CURVE('',#3827,#3828,#2157,.T.);
#4789=EDGE_CURVE('',#3691,#3829,#2158,.T.);
#4790=EDGE_CURVE('',#3828,#3829,#2159,.T.);
#4791=EDGE_CURVE('',#3690,#3830,#2160,.T.);
#4792=EDGE_CURVE('',#3829,#3830,#2161,.T.);
#4793=EDGE_CURVE('',#3831,#3689,#2162,.T.);
#4794=EDGE_CURVE('',#3830,#3831,#2163,.T.);
#4795=EDGE_CURVE('',#3832,#3833,#2164,.T.);
#4796=EDGE_CURVE('',#3833,#3834,#2165,.T.);
#4797=EDGE_CURVE('',#3834,#3835,#2166,.T.);
#4798=EDGE_CURVE('',#3835,#3836,#2167,.T.);
#4799=EDGE_CURVE('',#3836,#3837,#2168,.T.);
#4800=EDGE_CURVE('',#3837,#3826,#2169,.T.);
#4801=EDGE_CURVE('',#3823,#3838,#2170,.T.);
#4802=EDGE_CURVE('',#3838,#3839,#2171,.T.);
#4803=EDGE_CURVE('',#3839,#3840,#2172,.T.);
#4804=EDGE_CURVE('',#3840,#3841,#2173,.T.);
#4805=EDGE_CURVE('',#3841,#3842,#2174,.T.);
#4806=EDGE_CURVE('',#3842,#3832,#2175,.T.);
#4807=EDGE_CURVE('',#3834,#3625,#2176,.T.);
#4808=EDGE_CURVE('',#3626,#3833,#2177,.T.);
#4809=EDGE_CURVE('',#3835,#3624,#2178,.T.);
#4810=EDGE_CURVE('',#3836,#3623,#2179,.T.);
#4811=EDGE_CURVE('',#3837,#3622,#2180,.T.);
#4812=EDGE_CURVE('',#3843,#3822,#2181,.T.);
#4813=EDGE_CURVE('',#3838,#3843,#2182,.T.);
#4814=EDGE_CURVE('',#3844,#3843,#2183,.T.);
#4815=EDGE_CURVE('',#3839,#3844,#2184,.T.);
#4816=EDGE_CURVE('',#3845,#3844,#2185,.T.);
#4817=EDGE_CURVE('',#3840,#3845,#2186,.T.);
#4818=EDGE_CURVE('',#3846,#3845,#2187,.T.);
#4819=EDGE_CURVE('',#3841,#3846,#2188,.T.);
#4820=EDGE_CURVE('',#3847,#3846,#2189,.T.);
#4821=EDGE_CURVE('',#3842,#3847,#2190,.T.);
#4822=EDGE_CURVE('',#3848,#3847,#2191,.T.);
#4823=EDGE_CURVE('',#3832,#3848,#2192,.T.);
#4824=EDGE_CURVE('',#3831,#3848,#2193,.T.);
#4825=EDGE_CURVE('',#3667,#3849,#2194,.T.);
#4826=EDGE_CURVE('',#3850,#3849,#2195,.T.);
#4827=EDGE_CURVE('',#3851,#3850,#2196,.T.);
#4828=EDGE_CURVE('',#3852,#3851,#2197,.T.);
#4829=EDGE_CURVE('',#3852,#3601,#2198,.T.);
#4830=EDGE_CURVE('',#3708,#3853,#2199,.T.);
#4831=EDGE_CURVE('',#3849,#3853,#2200,.T.);
#4832=EDGE_CURVE('',#3854,#3852,#2201,.T.);
#4833=EDGE_CURVE('',#3854,#3603,#2202,.T.);
#4834=EDGE_CURVE('',#3707,#3855,#2203,.T.);
#4835=EDGE_CURVE('',#3853,#3855,#2204,.T.);
#4836=EDGE_CURVE('',#3706,#3856,#2205,.T.);
#4837=EDGE_CURVE('',#3855,#3856,#2206,.T.);
#4838=EDGE_CURVE('',#3705,#3857,#2207,.T.);
#4839=EDGE_CURVE('',#3856,#3857,#2208,.T.);
#4840=EDGE_CURVE('',#3704,#3858,#2209,.T.);
#4841=EDGE_CURVE('',#3857,#3858,#2210,.T.);
#4842=EDGE_CURVE('',#3859,#3703,#2211,.T.);
#4843=EDGE_CURVE('',#3858,#3859,#2212,.T.);
#4844=EDGE_CURVE('',#3860,#3861,#2213,.T.);
#4845=EDGE_CURVE('',#3861,#3862,#2214,.T.);
#4846=EDGE_CURVE('',#3862,#3863,#2215,.T.);
#4847=EDGE_CURVE('',#3863,#3864,#2216,.T.);
#4848=EDGE_CURVE('',#3864,#3865,#2217,.T.);
#4849=EDGE_CURVE('',#3865,#3854,#2218,.T.);
#4850=EDGE_CURVE('',#3851,#3866,#2219,.T.);
#4851=EDGE_CURVE('',#3866,#3867,#2220,.T.);
#4852=EDGE_CURVE('',#3867,#3868,#2221,.T.);
#4853=EDGE_CURVE('',#3868,#3869,#2222,.T.);
#4854=EDGE_CURVE('',#3869,#3870,#2223,.T.);
#4855=EDGE_CURVE('',#3870,#3860,#2224,.T.);
#4856=EDGE_CURVE('',#3862,#3607,#2225,.T.);
#4857=EDGE_CURVE('',#3608,#3861,#2226,.T.);
#4858=EDGE_CURVE('',#3863,#3606,#2227,.T.);
#4859=EDGE_CURVE('',#3864,#3605,#2228,.T.);
#4860=EDGE_CURVE('',#3865,#3604,#2229,.T.);
#4861=EDGE_CURVE('',#3871,#3850,#2230,.T.);
#4862=EDGE_CURVE('',#3866,#3871,#2231,.T.);
#4863=EDGE_CURVE('',#3872,#3871,#2232,.T.);
#4864=EDGE_CURVE('',#3867,#3872,#2233,.T.);
#4865=EDGE_CURVE('',#3873,#3872,#2234,.T.);
#4866=EDGE_CURVE('',#3868,#3873,#2235,.T.);
#4867=EDGE_CURVE('',#3874,#3873,#2236,.T.);
#4868=EDGE_CURVE('',#3869,#3874,#2237,.T.);
#4869=EDGE_CURVE('',#3875,#3874,#2238,.T.);
#4870=EDGE_CURVE('',#3870,#3875,#2239,.T.);
#4871=EDGE_CURVE('',#3876,#3875,#2240,.T.);
#4872=EDGE_CURVE('',#3860,#3876,#2241,.T.);
#4873=EDGE_CURVE('',#3859,#3876,#2242,.T.);
#4874=EDGE_CURVE('',#3877,#3878,#2243,.T.);
#4875=EDGE_CURVE('',#3877,#3879,#2244,.T.);
#4876=EDGE_CURVE('',#3879,#3880,#2245,.T.);
#4877=EDGE_CURVE('',#3878,#3880,#2246,.T.);
#4878=EDGE_CURVE('',#3881,#3877,#2247,.T.);
#4879=EDGE_CURVE('',#3881,#3882,#2248,.T.);
#4880=EDGE_CURVE('',#3882,#3879,#2249,.T.);
#4881=EDGE_CURVE('',#3883,#3881,#2250,.T.);
#4882=EDGE_CURVE('',#3883,#3884,#2251,.T.);
#4883=EDGE_CURVE('',#3884,#3882,#2252,.T.);
#4884=EDGE_CURVE('',#3885,#3883,#2253,.T.);
#4885=EDGE_CURVE('',#3885,#3886,#2254,.T.);
#4886=EDGE_CURVE('',#3886,#3884,#2255,.T.);
#4887=EDGE_CURVE('',#3887,#3885,#2256,.T.);
#4888=EDGE_CURVE('',#3887,#3888,#2257,.T.);
#4889=EDGE_CURVE('',#3888,#3886,#2258,.T.);
#4890=EDGE_CURVE('',#3878,#3887,#2259,.T.);
#4891=EDGE_CURVE('',#3880,#3888,#2260,.T.);
#4892=EDGE_CURVE('',#3889,#3889,#3257,.T.);
#4893=EDGE_CURVE('',#3890,#3890,#3258,.T.);
#4894=EDGE_CURVE('',#3890,#3889,#2261,.T.);
#4895=EDGE_CURVE('',#3891,#3891,#3259,.F.);
#4896=EDGE_CURVE('',#3891,#3890,#2262,.T.);
#4897=EDGE_CURVE('',#3892,#3892,#3260,.T.);
#4898=EDGE_CURVE('',#3892,#3891,#2263,.T.);
#4899=ORIENTED_EDGE('',*,*,#3893,.F.);
#4900=ORIENTED_EDGE('',*,*,#3894,.T.);
#4901=ORIENTED_EDGE('',*,*,#3895,.F.);
#4902=ORIENTED_EDGE('',*,*,#3894,.F.);
#4903=ORIENTED_EDGE('',*,*,#3896,.F.);
#4904=ORIENTED_EDGE('',*,*,#3897,.T.);
#4905=ORIENTED_EDGE('',*,*,#3898,.F.);
#4906=ORIENTED_EDGE('',*,*,#3897,.F.);
#4907=ORIENTED_EDGE('',*,*,#3899,.F.);
#4908=ORIENTED_EDGE('',*,*,#3900,.T.);
#4909=ORIENTED_EDGE('',*,*,#3901,.F.);
#4910=ORIENTED_EDGE('',*,*,#3900,.F.);
#4911=ORIENTED_EDGE('',*,*,#3902,.F.);
#4912=ORIENTED_EDGE('',*,*,#3903,.T.);
#4913=ORIENTED_EDGE('',*,*,#3904,.F.);
#4914=ORIENTED_EDGE('',*,*,#3903,.F.);
#4915=ORIENTED_EDGE('',*,*,#3905,.T.);
#4916=ORIENTED_EDGE('',*,*,#3906,.T.);
#4917=ORIENTED_EDGE('',*,*,#3907,.F.);
#4918=ORIENTED_EDGE('',*,*,#3908,.F.);
#4919=ORIENTED_EDGE('',*,*,#3909,.T.);
#4920=ORIENTED_EDGE('',*,*,#3908,.T.);
#4921=ORIENTED_EDGE('',*,*,#3910,.F.);
#4922=ORIENTED_EDGE('',*,*,#3911,.F.);
#4923=ORIENTED_EDGE('',*,*,#3912,.T.);
#4924=ORIENTED_EDGE('',*,*,#3911,.T.);
#4925=ORIENTED_EDGE('',*,*,#3913,.F.);
#4926=ORIENTED_EDGE('',*,*,#3914,.F.);
#4927=ORIENTED_EDGE('',*,*,#3915,.T.);
#4928=ORIENTED_EDGE('',*,*,#3914,.T.);
#4929=ORIENTED_EDGE('',*,*,#3916,.F.);
#4930=ORIENTED_EDGE('',*,*,#3906,.F.);
#4931=ORIENTED_EDGE('',*,*,#3916,.T.);
#4932=ORIENTED_EDGE('',*,*,#3913,.T.);
#4933=ORIENTED_EDGE('',*,*,#3910,.T.);
#4934=ORIENTED_EDGE('',*,*,#3907,.T.);
#4935=ORIENTED_EDGE('',*,*,#3895,.T.);
#4936=ORIENTED_EDGE('',*,*,#3898,.T.);
#4937=ORIENTED_EDGE('',*,*,#3901,.T.);
#4938=ORIENTED_EDGE('',*,*,#3904,.T.);
#4939=ORIENTED_EDGE('',*,*,#3915,.F.);
#4940=ORIENTED_EDGE('',*,*,#3905,.F.);
#4941=ORIENTED_EDGE('',*,*,#3909,.F.);
#4942=ORIENTED_EDGE('',*,*,#3912,.F.);
#4943=ORIENTED_EDGE('',*,*,#3893,.T.);
#4944=ORIENTED_EDGE('',*,*,#3896,.T.);
#4945=ORIENTED_EDGE('',*,*,#3899,.T.);
#4946=ORIENTED_EDGE('',*,*,#3902,.T.);
#4947=ORIENTED_EDGE('',*,*,#3917,.F.);
#4948=ORIENTED_EDGE('',*,*,#3918,.T.);
#4949=ORIENTED_EDGE('',*,*,#3919,.T.);
#4950=ORIENTED_EDGE('',*,*,#3918,.F.);
#4951=ORIENTED_EDGE('',*,*,#3917,.T.);
#4952=ORIENTED_EDGE('',*,*,#3919,.F.);
#4953=ORIENTED_EDGE('',*,*,#3920,.F.);
#4954=ORIENTED_EDGE('',*,*,#3921,.T.);
#4955=ORIENTED_EDGE('',*,*,#3922,.T.);
#4956=ORIENTED_EDGE('',*,*,#3921,.F.);
#4957=ORIENTED_EDGE('',*,*,#3920,.T.);
#4958=ORIENTED_EDGE('',*,*,#3922,.F.);
#4959=ORIENTED_EDGE('',*,*,#3923,.F.);
#4960=ORIENTED_EDGE('',*,*,#3924,.F.);
#4961=ORIENTED_EDGE('',*,*,#3925,.F.);
#4962=ORIENTED_EDGE('',*,*,#3926,.F.);
#4963=ORIENTED_EDGE('',*,*,#3927,.F.);
#4964=ORIENTED_EDGE('',*,*,#3924,.T.);
#4965=ORIENTED_EDGE('',*,*,#3928,.F.);
#4966=ORIENTED_EDGE('',*,*,#3929,.T.);
#4967=ORIENTED_EDGE('',*,*,#3930,.F.);
#4968=ORIENTED_EDGE('',*,*,#3931,.F.);
#4969=ORIENTED_EDGE('',*,*,#3932,.F.);
#4970=ORIENTED_EDGE('',*,*,#3929,.F.);
#4971=ORIENTED_EDGE('',*,*,#3933,.T.);
#4972=ORIENTED_EDGE('',*,*,#3934,.F.);
#4973=ORIENTED_EDGE('',*,*,#3935,.T.);
#4974=ORIENTED_EDGE('',*,*,#3936,.F.);
#4975=ORIENTED_EDGE('',*,*,#3937,.T.);
#4976=ORIENTED_EDGE('',*,*,#3926,.T.);
#4977=ORIENTED_EDGE('',*,*,#3938,.T.);
#4978=ORIENTED_EDGE('',*,*,#3925,.T.);
#4979=ORIENTED_EDGE('',*,*,#3923,.T.);
#4980=ORIENTED_EDGE('',*,*,#3927,.T.);
#4981=ORIENTED_EDGE('',*,*,#3937,.F.);
#4982=ORIENTED_EDGE('',*,*,#3939,.F.);
#4983=ORIENTED_EDGE('',*,*,#3940,.T.);
#4984=ORIENTED_EDGE('',*,*,#3941,.F.);
#4985=ORIENTED_EDGE('',*,*,#3933,.F.);
#4986=ORIENTED_EDGE('',*,*,#3942,.T.);
#4987=ORIENTED_EDGE('',*,*,#3943,.T.);
#4988=ORIENTED_EDGE('',*,*,#3944,.F.);
#4989=ORIENTED_EDGE('',*,*,#3945,.F.);
#4990=ORIENTED_EDGE('',*,*,#3931,.T.);
#4991=ORIENTED_EDGE('',*,*,#3946,.F.);
#4992=ORIENTED_EDGE('',*,*,#3947,.F.);
#4993=ORIENTED_EDGE('',*,*,#3948,.T.);
#4994=ORIENTED_EDGE('',*,*,#3949,.F.);
#4995=ORIENTED_EDGE('',*,*,#3950,.T.);
#4996=ORIENTED_EDGE('',*,*,#3951,.F.);
#4997=ORIENTED_EDGE('',*,*,#3950,.F.);
#4998=ORIENTED_EDGE('',*,*,#3942,.F.);
#4999=ORIENTED_EDGE('',*,*,#3952,.T.);
#5000=ORIENTED_EDGE('',*,*,#3953,.F.);
#5001=ORIENTED_EDGE('',*,*,#3952,.F.);
#5002=ORIENTED_EDGE('',*,*,#3954,.F.);
#5003=ORIENTED_EDGE('',*,*,#3955,.T.);
#5004=ORIENTED_EDGE('',*,*,#3938,.F.);
#5005=ORIENTED_EDGE('',*,*,#3955,.F.);
#5006=ORIENTED_EDGE('',*,*,#3956,.F.);
#5007=ORIENTED_EDGE('',*,*,#3957,.T.);
#5008=ORIENTED_EDGE('',*,*,#3948,.F.);
#5009=ORIENTED_EDGE('',*,*,#3957,.F.);
#5010=ORIENTED_EDGE('',*,*,#3958,.F.);
#5011=ORIENTED_EDGE('',*,*,#3959,.T.);
#5012=ORIENTED_EDGE('',*,*,#3960,.F.);
#5013=ORIENTED_EDGE('',*,*,#3959,.F.);
#5014=ORIENTED_EDGE('',*,*,#3936,.T.);
#5015=ORIENTED_EDGE('',*,*,#3961,.T.);
#5016=ORIENTED_EDGE('',*,*,#3962,.T.);
#5017=ORIENTED_EDGE('',*,*,#3963,.T.);
#5018=ORIENTED_EDGE('',*,*,#3947,.T.);
#5019=ORIENTED_EDGE('',*,*,#3964,.T.);
#5020=ORIENTED_EDGE('',*,*,#3965,.T.);
#5021=ORIENTED_EDGE('',*,*,#3966,.T.);
#5022=ORIENTED_EDGE('',*,*,#3967,.T.);
#5023=ORIENTED_EDGE('',*,*,#3968,.T.);
#5024=ORIENTED_EDGE('',*,*,#3969,.T.);
#5025=ORIENTED_EDGE('',*,*,#3939,.T.);
#5026=ORIENTED_EDGE('',*,*,#3958,.T.);
#5027=ORIENTED_EDGE('',*,*,#3935,.F.);
#5028=ORIENTED_EDGE('',*,*,#3970,.F.);
#5029=ORIENTED_EDGE('',*,*,#3971,.F.);
#5030=ORIENTED_EDGE('',*,*,#3961,.F.);
#5031=ORIENTED_EDGE('',*,*,#3971,.T.);
#5032=ORIENTED_EDGE('',*,*,#3972,.F.);
#5033=ORIENTED_EDGE('',*,*,#3973,.F.);
#5034=ORIENTED_EDGE('',*,*,#3962,.F.);
#5035=ORIENTED_EDGE('',*,*,#3954,.T.);
#5036=ORIENTED_EDGE('',*,*,#3956,.T.);
#5037=ORIENTED_EDGE('',*,*,#3973,.T.);
#5038=ORIENTED_EDGE('',*,*,#3974,.F.);
#5039=ORIENTED_EDGE('',*,*,#3943,.F.);
#5040=ORIENTED_EDGE('',*,*,#3963,.F.);
#5041=ORIENTED_EDGE('',*,*,#3928,.T.);
#5042=ORIENTED_EDGE('',*,*,#3945,.T.);
#5043=ORIENTED_EDGE('',*,*,#3975,.F.);
#5044=ORIENTED_EDGE('',*,*,#3976,.F.);
#5045=ORIENTED_EDGE('',*,*,#3964,.F.);
#5046=ORIENTED_EDGE('',*,*,#3946,.T.);
#5047=ORIENTED_EDGE('',*,*,#3930,.T.);
#5048=ORIENTED_EDGE('',*,*,#3932,.T.);
#5049=ORIENTED_EDGE('',*,*,#3951,.T.);
#5050=ORIENTED_EDGE('',*,*,#3976,.T.);
#5051=ORIENTED_EDGE('',*,*,#3977,.F.);
#5052=ORIENTED_EDGE('',*,*,#3978,.F.);
#5053=ORIENTED_EDGE('',*,*,#3965,.F.);
#5054=ORIENTED_EDGE('',*,*,#3978,.T.);
#5055=ORIENTED_EDGE('',*,*,#3979,.F.);
#5056=ORIENTED_EDGE('',*,*,#3980,.F.);
#5057=ORIENTED_EDGE('',*,*,#3966,.F.);
#5058=ORIENTED_EDGE('',*,*,#3949,.T.);
#5059=ORIENTED_EDGE('',*,*,#3980,.T.);
#5060=ORIENTED_EDGE('',*,*,#3981,.F.);
#5061=ORIENTED_EDGE('',*,*,#3982,.F.);
#5062=ORIENTED_EDGE('',*,*,#3967,.F.);
#5063=ORIENTED_EDGE('',*,*,#3982,.T.);
#5064=ORIENTED_EDGE('',*,*,#3983,.F.);
#5065=ORIENTED_EDGE('',*,*,#3984,.F.);
#5066=ORIENTED_EDGE('',*,*,#3968,.F.);
#5067=ORIENTED_EDGE('',*,*,#3953,.T.);
#5068=ORIENTED_EDGE('',*,*,#3984,.T.);
#5069=ORIENTED_EDGE('',*,*,#3985,.F.);
#5070=ORIENTED_EDGE('',*,*,#3940,.F.);
#5071=ORIENTED_EDGE('',*,*,#3969,.F.);
#5072=ORIENTED_EDGE('',*,*,#3934,.T.);
#5073=ORIENTED_EDGE('',*,*,#3941,.T.);
#5074=ORIENTED_EDGE('',*,*,#3985,.T.);
#5075=ORIENTED_EDGE('',*,*,#3983,.T.);
#5076=ORIENTED_EDGE('',*,*,#3981,.T.);
#5077=ORIENTED_EDGE('',*,*,#3979,.T.);
#5078=ORIENTED_EDGE('',*,*,#3977,.T.);
#5079=ORIENTED_EDGE('',*,*,#3975,.T.);
#5080=ORIENTED_EDGE('',*,*,#3944,.T.);
#5081=ORIENTED_EDGE('',*,*,#3974,.T.);
#5082=ORIENTED_EDGE('',*,*,#3972,.T.);
#5083=ORIENTED_EDGE('',*,*,#3970,.T.);
#5084=ORIENTED_EDGE('',*,*,#3960,.T.);
#5085=ORIENTED_EDGE('',*,*,#3986,.T.);
#5086=ORIENTED_EDGE('',*,*,#3987,.T.);
#5087=ORIENTED_EDGE('',*,*,#3988,.T.);
#5088=ORIENTED_EDGE('',*,*,#3989,.F.);
#5089=ORIENTED_EDGE('',*,*,#3990,.T.);
#5090=ORIENTED_EDGE('',*,*,#3991,.T.);
#5091=ORIENTED_EDGE('',*,*,#3992,.T.);
#5092=ORIENTED_EDGE('',*,*,#3987,.F.);
#5093=ORIENTED_EDGE('',*,*,#3993,.T.);
#5094=ORIENTED_EDGE('',*,*,#3994,.T.);
#5095=ORIENTED_EDGE('',*,*,#3995,.T.);
#5096=ORIENTED_EDGE('',*,*,#3991,.F.);
#5097=ORIENTED_EDGE('',*,*,#3996,.T.);
#5098=ORIENTED_EDGE('',*,*,#3997,.T.);
#5099=ORIENTED_EDGE('',*,*,#3998,.T.);
#5100=ORIENTED_EDGE('',*,*,#3994,.F.);
#5101=ORIENTED_EDGE('',*,*,#3999,.T.);
#5102=ORIENTED_EDGE('',*,*,#4000,.T.);
#5103=ORIENTED_EDGE('',*,*,#4001,.T.);
#5104=ORIENTED_EDGE('',*,*,#3997,.F.);
#5105=ORIENTED_EDGE('',*,*,#4002,.T.);
#5106=ORIENTED_EDGE('',*,*,#3989,.T.);
#5107=ORIENTED_EDGE('',*,*,#4003,.T.);
#5108=ORIENTED_EDGE('',*,*,#4000,.F.);
#5109=ORIENTED_EDGE('',*,*,#4002,.F.);
#5110=ORIENTED_EDGE('',*,*,#3999,.F.);
#5111=ORIENTED_EDGE('',*,*,#3996,.F.);
#5112=ORIENTED_EDGE('',*,*,#3993,.F.);
#5113=ORIENTED_EDGE('',*,*,#3990,.F.);
#5114=ORIENTED_EDGE('',*,*,#3986,.F.);
#5115=ORIENTED_EDGE('',*,*,#4003,.F.);
#5116=ORIENTED_EDGE('',*,*,#3988,.F.);
#5117=ORIENTED_EDGE('',*,*,#3992,.F.);
#5118=ORIENTED_EDGE('',*,*,#3995,.F.);
#5119=ORIENTED_EDGE('',*,*,#3998,.F.);
#5120=ORIENTED_EDGE('',*,*,#4001,.F.);
#5121=ORIENTED_EDGE('',*,*,#4004,.F.);
#5122=ORIENTED_EDGE('',*,*,#4005,.F.);
#5123=ORIENTED_EDGE('',*,*,#4006,.F.);
#5124=ORIENTED_EDGE('',*,*,#4007,.T.);
#5125=ORIENTED_EDGE('',*,*,#4005,.T.);
#5126=ORIENTED_EDGE('',*,*,#4007,.F.);
#5127=ORIENTED_EDGE('',*,*,#4008,.F.);
#5128=ORIENTED_EDGE('',*,*,#4009,.T.);
#5129=ORIENTED_EDGE('',*,*,#4006,.T.);
#5130=ORIENTED_EDGE('',*,*,#4009,.F.);
#5131=ORIENTED_EDGE('',*,*,#4010,.F.);
#5132=ORIENTED_EDGE('',*,*,#4011,.T.);
#5133=ORIENTED_EDGE('',*,*,#4008,.T.);
#5134=ORIENTED_EDGE('',*,*,#4011,.F.);
#5135=ORIENTED_EDGE('',*,*,#4010,.T.);
#5136=ORIENTED_EDGE('',*,*,#4012,.F.);
#5137=ORIENTED_EDGE('',*,*,#4013,.F.);
#5138=ORIENTED_EDGE('',*,*,#4014,.T.);
#5139=ORIENTED_EDGE('',*,*,#4012,.T.);
#5140=ORIENTED_EDGE('',*,*,#4014,.F.);
#5141=ORIENTED_EDGE('',*,*,#4004,.T.);
#5142=ORIENTED_EDGE('',*,*,#4015,.T.);
#5143=ORIENTED_EDGE('',*,*,#4013,.T.);
#5144=ORIENTED_EDGE('',*,*,#4015,.F.);
#5145=ORIENTED_EDGE('',*,*,#4016,.F.);
#5146=ORIENTED_EDGE('',*,*,#4017,.F.);
#5147=ORIENTED_EDGE('',*,*,#4018,.T.);
#5148=ORIENTED_EDGE('',*,*,#4016,.T.);
#5149=ORIENTED_EDGE('',*,*,#4018,.F.);
#5150=ORIENTED_EDGE('',*,*,#4019,.F.);
#5151=ORIENTED_EDGE('',*,*,#4020,.T.);
#5152=ORIENTED_EDGE('',*,*,#4017,.T.);
#5153=ORIENTED_EDGE('',*,*,#4020,.F.);
#5154=ORIENTED_EDGE('',*,*,#4021,.F.);
#5155=ORIENTED_EDGE('',*,*,#4022,.T.);
#5156=ORIENTED_EDGE('',*,*,#4019,.T.);
#5157=ORIENTED_EDGE('',*,*,#4022,.F.);
#5158=ORIENTED_EDGE('',*,*,#4021,.T.);
#5159=ORIENTED_EDGE('',*,*,#4023,.F.);
#5160=ORIENTED_EDGE('',*,*,#4024,.F.);
#5161=ORIENTED_EDGE('',*,*,#4025,.T.);
#5162=ORIENTED_EDGE('',*,*,#4023,.T.);
#5163=ORIENTED_EDGE('',*,*,#4025,.F.);
#5164=ORIENTED_EDGE('',*,*,#4026,.F.);
#5165=ORIENTED_EDGE('',*,*,#4027,.T.);
#5166=ORIENTED_EDGE('',*,*,#4024,.T.);
#5167=ORIENTED_EDGE('',*,*,#4027,.F.);
#5168=ORIENTED_EDGE('',*,*,#4028,.F.);
#5169=ORIENTED_EDGE('',*,*,#4029,.T.);
#5170=ORIENTED_EDGE('',*,*,#4026,.T.);
#5171=ORIENTED_EDGE('',*,*,#4029,.F.);
#5172=ORIENTED_EDGE('',*,*,#4028,.T.);
#5173=ORIENTED_EDGE('',*,*,#4030,.T.);
#5174=ORIENTED_EDGE('',*,*,#4031,.T.);
#5175=ORIENTED_EDGE('',*,*,#4032,.T.);
#5176=ORIENTED_EDGE('',*,*,#4033,.F.);
#5177=ORIENTED_EDGE('',*,*,#4034,.T.);
#5178=ORIENTED_EDGE('',*,*,#4035,.T.);
#5179=ORIENTED_EDGE('',*,*,#4036,.T.);
#5180=ORIENTED_EDGE('',*,*,#4031,.F.);
#5181=ORIENTED_EDGE('',*,*,#4037,.T.);
#5182=ORIENTED_EDGE('',*,*,#4038,.T.);
#5183=ORIENTED_EDGE('',*,*,#4039,.T.);
#5184=ORIENTED_EDGE('',*,*,#4035,.F.);
#5185=ORIENTED_EDGE('',*,*,#4040,.T.);
#5186=ORIENTED_EDGE('',*,*,#4041,.T.);
#5187=ORIENTED_EDGE('',*,*,#4042,.T.);
#5188=ORIENTED_EDGE('',*,*,#4038,.F.);
#5189=ORIENTED_EDGE('',*,*,#4043,.T.);
#5190=ORIENTED_EDGE('',*,*,#4044,.T.);
#5191=ORIENTED_EDGE('',*,*,#4045,.T.);
#5192=ORIENTED_EDGE('',*,*,#4041,.F.);
#5193=ORIENTED_EDGE('',*,*,#4046,.T.);
#5194=ORIENTED_EDGE('',*,*,#4033,.T.);
#5195=ORIENTED_EDGE('',*,*,#4047,.T.);
#5196=ORIENTED_EDGE('',*,*,#4044,.F.);
#5197=ORIENTED_EDGE('',*,*,#4046,.F.);
#5198=ORIENTED_EDGE('',*,*,#4043,.F.);
#5199=ORIENTED_EDGE('',*,*,#4040,.F.);
#5200=ORIENTED_EDGE('',*,*,#4037,.F.);
#5201=ORIENTED_EDGE('',*,*,#4034,.F.);
#5202=ORIENTED_EDGE('',*,*,#4030,.F.);
#5203=ORIENTED_EDGE('',*,*,#4047,.F.);
#5204=ORIENTED_EDGE('',*,*,#4032,.F.);
#5205=ORIENTED_EDGE('',*,*,#4036,.F.);
#5206=ORIENTED_EDGE('',*,*,#4039,.F.);
#5207=ORIENTED_EDGE('',*,*,#4042,.F.);
#5208=ORIENTED_EDGE('',*,*,#4045,.F.);
#5209=ORIENTED_EDGE('',*,*,#4048,.F.);
#5210=ORIENTED_EDGE('',*,*,#4049,.T.);
#5211=ORIENTED_EDGE('',*,*,#4050,.F.);
#5212=ORIENTED_EDGE('',*,*,#4049,.F.);
#5213=ORIENTED_EDGE('',*,*,#4051,.F.);
#5214=ORIENTED_EDGE('',*,*,#4052,.T.);
#5215=ORIENTED_EDGE('',*,*,#4053,.F.);
#5216=ORIENTED_EDGE('',*,*,#4054,.T.);
#5217=ORIENTED_EDGE('',*,*,#4051,.T.);
#5218=ORIENTED_EDGE('',*,*,#4054,.F.);
#5219=ORIENTED_EDGE('',*,*,#4055,.F.);
#5220=ORIENTED_EDGE('',*,*,#4056,.T.);
#5221=ORIENTED_EDGE('',*,*,#4053,.T.);
#5222=ORIENTED_EDGE('',*,*,#4056,.F.);
#5223=ORIENTED_EDGE('',*,*,#4050,.T.);
#5224=ORIENTED_EDGE('',*,*,#4057,.F.);
#5225=ORIENTED_EDGE('',*,*,#4058,.T.);
#5226=ORIENTED_EDGE('',*,*,#4055,.T.);
#5227=ORIENTED_EDGE('',*,*,#4058,.F.);
#5228=ORIENTED_EDGE('',*,*,#4057,.T.);
#5229=ORIENTED_EDGE('',*,*,#4059,.F.);
#5230=ORIENTED_EDGE('',*,*,#4059,.T.);
#5231=ORIENTED_EDGE('',*,*,#4060,.T.);
#5232=ORIENTED_EDGE('',*,*,#4052,.F.);
#5233=ORIENTED_EDGE('',*,*,#4060,.F.);
#5234=ORIENTED_EDGE('',*,*,#4048,.T.);
#5235=ORIENTED_EDGE('',*,*,#4061,.F.);
#5236=ORIENTED_EDGE('',*,*,#4062,.F.);
#5237=ORIENTED_EDGE('',*,*,#4063,.T.);
#5238=ORIENTED_EDGE('',*,*,#4064,.F.);
#5239=ORIENTED_EDGE('',*,*,#4063,.F.);
#5240=ORIENTED_EDGE('',*,*,#4065,.F.);
#5241=ORIENTED_EDGE('',*,*,#4066,.T.);
#5242=ORIENTED_EDGE('',*,*,#4067,.F.);
#5243=ORIENTED_EDGE('',*,*,#4066,.F.);
#5244=ORIENTED_EDGE('',*,*,#4061,.T.);
#5245=ORIENTED_EDGE('',*,*,#4062,.T.);
#5246=ORIENTED_EDGE('',*,*,#4068,.F.);
#5247=ORIENTED_EDGE('',*,*,#4069,.T.);
#5248=ORIENTED_EDGE('',*,*,#4070,.F.);
#5249=ORIENTED_EDGE('',*,*,#4071,.F.);
#5250=ORIENTED_EDGE('',*,*,#4072,.F.);
#5251=ORIENTED_EDGE('',*,*,#4071,.T.);
#5252=ORIENTED_EDGE('',*,*,#4073,.F.);
#5253=ORIENTED_EDGE('',*,*,#4074,.F.);
#5254=ORIENTED_EDGE('',*,*,#4075,.F.);
#5255=ORIENTED_EDGE('',*,*,#4074,.T.);
#5256=ORIENTED_EDGE('',*,*,#4076,.F.);
#5257=ORIENTED_EDGE('',*,*,#4077,.F.);
#5258=ORIENTED_EDGE('',*,*,#4078,.F.);
#5259=ORIENTED_EDGE('',*,*,#4077,.T.);
#5260=ORIENTED_EDGE('',*,*,#4079,.F.);
#5261=ORIENTED_EDGE('',*,*,#4080,.F.);
#5262=ORIENTED_EDGE('',*,*,#4081,.F.);
#5263=ORIENTED_EDGE('',*,*,#4080,.T.);
#5264=ORIENTED_EDGE('',*,*,#4082,.F.);
#5265=ORIENTED_EDGE('',*,*,#4083,.F.);
#5266=ORIENTED_EDGE('',*,*,#4084,.F.);
#5267=ORIENTED_EDGE('',*,*,#4083,.T.);
#5268=ORIENTED_EDGE('',*,*,#4085,.F.);
#5269=ORIENTED_EDGE('',*,*,#4086,.F.);
#5270=ORIENTED_EDGE('',*,*,#4087,.F.);
#5271=ORIENTED_EDGE('',*,*,#4086,.T.);
#5272=ORIENTED_EDGE('',*,*,#4088,.F.);
#5273=ORIENTED_EDGE('',*,*,#4089,.F.);
#5274=ORIENTED_EDGE('',*,*,#4090,.F.);
#5275=ORIENTED_EDGE('',*,*,#4089,.T.);
#5276=ORIENTED_EDGE('',*,*,#4091,.F.);
#5277=ORIENTED_EDGE('',*,*,#4092,.F.);
#5278=ORIENTED_EDGE('',*,*,#4093,.F.);
#5279=ORIENTED_EDGE('',*,*,#4092,.T.);
#5280=ORIENTED_EDGE('',*,*,#4094,.F.);
#5281=ORIENTED_EDGE('',*,*,#4095,.F.);
#5282=ORIENTED_EDGE('',*,*,#4096,.F.);
#5283=ORIENTED_EDGE('',*,*,#4095,.T.);
#5284=ORIENTED_EDGE('',*,*,#4097,.F.);
#5285=ORIENTED_EDGE('',*,*,#4098,.F.);
#5286=ORIENTED_EDGE('',*,*,#4099,.F.);
#5287=ORIENTED_EDGE('',*,*,#4098,.T.);
#5288=ORIENTED_EDGE('',*,*,#4100,.F.);
#5289=ORIENTED_EDGE('',*,*,#4101,.F.);
#5290=ORIENTED_EDGE('',*,*,#4102,.F.);
#5291=ORIENTED_EDGE('',*,*,#4101,.T.);
#5292=ORIENTED_EDGE('',*,*,#4103,.F.);
#5293=ORIENTED_EDGE('',*,*,#4104,.F.);
#5294=ORIENTED_EDGE('',*,*,#4105,.F.);
#5295=ORIENTED_EDGE('',*,*,#4104,.T.);
#5296=ORIENTED_EDGE('',*,*,#4106,.F.);
#5297=ORIENTED_EDGE('',*,*,#4107,.F.);
#5298=ORIENTED_EDGE('',*,*,#4108,.F.);
#5299=ORIENTED_EDGE('',*,*,#4107,.T.);
#5300=ORIENTED_EDGE('',*,*,#4109,.F.);
#5301=ORIENTED_EDGE('',*,*,#4110,.F.);
#5302=ORIENTED_EDGE('',*,*,#4111,.F.);
#5303=ORIENTED_EDGE('',*,*,#4110,.T.);
#5304=ORIENTED_EDGE('',*,*,#4112,.F.);
#5305=ORIENTED_EDGE('',*,*,#4113,.F.);
#5306=ORIENTED_EDGE('',*,*,#4114,.F.);
#5307=ORIENTED_EDGE('',*,*,#4113,.T.);
#5308=ORIENTED_EDGE('',*,*,#4115,.F.);
#5309=ORIENTED_EDGE('',*,*,#4116,.F.);
#5310=ORIENTED_EDGE('',*,*,#4117,.F.);
#5311=ORIENTED_EDGE('',*,*,#4116,.T.);
#5312=ORIENTED_EDGE('',*,*,#4118,.F.);
#5313=ORIENTED_EDGE('',*,*,#4119,.F.);
#5314=ORIENTED_EDGE('',*,*,#4120,.F.);
#5315=ORIENTED_EDGE('',*,*,#4119,.T.);
#5316=ORIENTED_EDGE('',*,*,#4121,.F.);
#5317=ORIENTED_EDGE('',*,*,#4069,.F.);
#5318=ORIENTED_EDGE('',*,*,#4120,.T.);
#5319=ORIENTED_EDGE('',*,*,#4068,.T.);
#5320=ORIENTED_EDGE('',*,*,#4072,.T.);
#5321=ORIENTED_EDGE('',*,*,#4075,.T.);
#5322=ORIENTED_EDGE('',*,*,#4078,.T.);
#5323=ORIENTED_EDGE('',*,*,#4081,.T.);
#5324=ORIENTED_EDGE('',*,*,#4084,.T.);
#5325=ORIENTED_EDGE('',*,*,#4087,.T.);
#5326=ORIENTED_EDGE('',*,*,#4090,.T.);
#5327=ORIENTED_EDGE('',*,*,#4093,.T.);
#5328=ORIENTED_EDGE('',*,*,#4096,.T.);
#5329=ORIENTED_EDGE('',*,*,#4099,.T.);
#5330=ORIENTED_EDGE('',*,*,#4102,.T.);
#5331=ORIENTED_EDGE('',*,*,#4105,.T.);
#5332=ORIENTED_EDGE('',*,*,#4108,.T.);
#5333=ORIENTED_EDGE('',*,*,#4111,.T.);
#5334=ORIENTED_EDGE('',*,*,#4114,.T.);
#5335=ORIENTED_EDGE('',*,*,#4117,.T.);
#5336=ORIENTED_EDGE('',*,*,#4070,.T.);
#5337=ORIENTED_EDGE('',*,*,#4122,.T.);
#5338=ORIENTED_EDGE('',*,*,#4073,.T.);
#5339=ORIENTED_EDGE('',*,*,#4123,.T.);
#5340=ORIENTED_EDGE('',*,*,#4076,.T.);
#5341=ORIENTED_EDGE('',*,*,#4124,.T.);
#5342=ORIENTED_EDGE('',*,*,#4079,.T.);
#5343=ORIENTED_EDGE('',*,*,#4125,.T.);
#5344=ORIENTED_EDGE('',*,*,#4082,.T.);
#5345=ORIENTED_EDGE('',*,*,#4126,.T.);
#5346=ORIENTED_EDGE('',*,*,#4085,.T.);
#5347=ORIENTED_EDGE('',*,*,#4127,.T.);
#5348=ORIENTED_EDGE('',*,*,#4088,.T.);
#5349=ORIENTED_EDGE('',*,*,#4128,.T.);
#5350=ORIENTED_EDGE('',*,*,#4091,.T.);
#5351=ORIENTED_EDGE('',*,*,#4129,.T.);
#5352=ORIENTED_EDGE('',*,*,#4094,.T.);
#5353=ORIENTED_EDGE('',*,*,#4130,.T.);
#5354=ORIENTED_EDGE('',*,*,#4131,.T.);
#5355=ORIENTED_EDGE('',*,*,#4132,.T.);
#5356=ORIENTED_EDGE('',*,*,#4133,.T.);
#5357=ORIENTED_EDGE('',*,*,#4134,.T.);
#5358=ORIENTED_EDGE('',*,*,#4135,.T.);
#5359=ORIENTED_EDGE('',*,*,#4136,.T.);
#5360=ORIENTED_EDGE('',*,*,#4137,.T.);
#5361=ORIENTED_EDGE('',*,*,#4138,.T.);
#5362=ORIENTED_EDGE('',*,*,#4139,.T.);
#5363=ORIENTED_EDGE('',*,*,#4140,.T.);
#5364=ORIENTED_EDGE('',*,*,#4141,.T.);
#5365=ORIENTED_EDGE('',*,*,#4142,.T.);
#5366=ORIENTED_EDGE('',*,*,#4143,.T.);
#5367=ORIENTED_EDGE('',*,*,#4144,.T.);
#5368=ORIENTED_EDGE('',*,*,#4145,.T.);
#5369=ORIENTED_EDGE('',*,*,#4146,.T.);
#5370=ORIENTED_EDGE('',*,*,#4147,.T.);
#5371=ORIENTED_EDGE('',*,*,#4148,.T.);
#5372=ORIENTED_EDGE('',*,*,#4149,.T.);
#5373=ORIENTED_EDGE('',*,*,#4150,.T.);
#5374=ORIENTED_EDGE('',*,*,#4151,.T.);
#5375=ORIENTED_EDGE('',*,*,#4152,.T.);
#5376=ORIENTED_EDGE('',*,*,#4153,.T.);
#5377=ORIENTED_EDGE('',*,*,#4121,.T.);
#5378=ORIENTED_EDGE('',*,*,#4118,.T.);
#5379=ORIENTED_EDGE('',*,*,#4115,.T.);
#5380=ORIENTED_EDGE('',*,*,#4112,.T.);
#5381=ORIENTED_EDGE('',*,*,#4109,.T.);
#5382=ORIENTED_EDGE('',*,*,#4106,.T.);
#5383=ORIENTED_EDGE('',*,*,#4103,.T.);
#5384=ORIENTED_EDGE('',*,*,#4100,.T.);
#5385=ORIENTED_EDGE('',*,*,#4097,.T.);
#5386=ORIENTED_EDGE('',*,*,#4067,.T.);
#5387=ORIENTED_EDGE('',*,*,#4154,.F.);
#5388=ORIENTED_EDGE('',*,*,#4155,.T.);
#5389=ORIENTED_EDGE('',*,*,#4156,.F.);
#5390=ORIENTED_EDGE('',*,*,#4157,.F.);
#5391=ORIENTED_EDGE('',*,*,#4158,.F.);
#5392=ORIENTED_EDGE('',*,*,#4157,.T.);
#5393=ORIENTED_EDGE('',*,*,#4159,.F.);
#5394=ORIENTED_EDGE('',*,*,#4160,.F.);
#5395=ORIENTED_EDGE('',*,*,#4161,.F.);
#5396=ORIENTED_EDGE('',*,*,#4160,.T.);
#5397=ORIENTED_EDGE('',*,*,#4162,.F.);
#5398=ORIENTED_EDGE('',*,*,#4163,.F.);
#5399=ORIENTED_EDGE('',*,*,#4164,.F.);
#5400=ORIENTED_EDGE('',*,*,#4163,.T.);
#5401=ORIENTED_EDGE('',*,*,#4165,.F.);
#5402=ORIENTED_EDGE('',*,*,#4166,.F.);
#5403=ORIENTED_EDGE('',*,*,#4167,.F.);
#5404=ORIENTED_EDGE('',*,*,#4166,.T.);
#5405=ORIENTED_EDGE('',*,*,#4168,.F.);
#5406=ORIENTED_EDGE('',*,*,#4169,.F.);
#5407=ORIENTED_EDGE('',*,*,#4170,.F.);
#5408=ORIENTED_EDGE('',*,*,#4169,.T.);
#5409=ORIENTED_EDGE('',*,*,#4171,.F.);
#5410=ORIENTED_EDGE('',*,*,#4172,.F.);
#5411=ORIENTED_EDGE('',*,*,#4173,.F.);
#5412=ORIENTED_EDGE('',*,*,#4172,.T.);
#5413=ORIENTED_EDGE('',*,*,#4174,.F.);
#5414=ORIENTED_EDGE('',*,*,#4175,.F.);
#5415=ORIENTED_EDGE('',*,*,#4176,.F.);
#5416=ORIENTED_EDGE('',*,*,#4175,.T.);
#5417=ORIENTED_EDGE('',*,*,#4177,.F.);
#5418=ORIENTED_EDGE('',*,*,#4178,.F.);
#5419=ORIENTED_EDGE('',*,*,#4179,.F.);
#5420=ORIENTED_EDGE('',*,*,#4178,.T.);
#5421=ORIENTED_EDGE('',*,*,#4151,.F.);
#5422=ORIENTED_EDGE('',*,*,#4180,.F.);
#5423=ORIENTED_EDGE('',*,*,#4181,.F.);
#5424=ORIENTED_EDGE('',*,*,#4180,.T.);
#5425=ORIENTED_EDGE('',*,*,#4150,.F.);
#5426=ORIENTED_EDGE('',*,*,#4182,.F.);
#5427=ORIENTED_EDGE('',*,*,#4183,.F.);
#5428=ORIENTED_EDGE('',*,*,#4182,.T.);
#5429=ORIENTED_EDGE('',*,*,#4149,.F.);
#5430=ORIENTED_EDGE('',*,*,#4184,.F.);
#5431=ORIENTED_EDGE('',*,*,#4185,.F.);
#5432=ORIENTED_EDGE('',*,*,#4184,.T.);
#5433=ORIENTED_EDGE('',*,*,#4148,.F.);
#5434=ORIENTED_EDGE('',*,*,#4186,.F.);
#5435=ORIENTED_EDGE('',*,*,#4187,.F.);
#5436=ORIENTED_EDGE('',*,*,#4186,.T.);
#5437=ORIENTED_EDGE('',*,*,#4147,.F.);
#5438=ORIENTED_EDGE('',*,*,#4188,.F.);
#5439=ORIENTED_EDGE('',*,*,#4189,.F.);
#5440=ORIENTED_EDGE('',*,*,#4188,.T.);
#5441=ORIENTED_EDGE('',*,*,#4146,.F.);
#5442=ORIENTED_EDGE('',*,*,#4190,.F.);
#5443=ORIENTED_EDGE('',*,*,#4191,.F.);
#5444=ORIENTED_EDGE('',*,*,#4190,.T.);
#5445=ORIENTED_EDGE('',*,*,#4145,.F.);
#5446=ORIENTED_EDGE('',*,*,#4192,.F.);
#5447=ORIENTED_EDGE('',*,*,#4193,.F.);
#5448=ORIENTED_EDGE('',*,*,#4192,.T.);
#5449=ORIENTED_EDGE('',*,*,#4144,.F.);
#5450=ORIENTED_EDGE('',*,*,#4194,.F.);
#5451=ORIENTED_EDGE('',*,*,#4195,.F.);
#5452=ORIENTED_EDGE('',*,*,#4194,.T.);
#5453=ORIENTED_EDGE('',*,*,#4143,.F.);
#5454=ORIENTED_EDGE('',*,*,#4196,.F.);
#5455=ORIENTED_EDGE('',*,*,#4197,.F.);
#5456=ORIENTED_EDGE('',*,*,#4196,.T.);
#5457=ORIENTED_EDGE('',*,*,#4142,.F.);
#5458=ORIENTED_EDGE('',*,*,#4155,.F.);
#5459=ORIENTED_EDGE('',*,*,#4197,.T.);
#5460=ORIENTED_EDGE('',*,*,#4154,.T.);
#5461=ORIENTED_EDGE('',*,*,#4158,.T.);
#5462=ORIENTED_EDGE('',*,*,#4161,.T.);
#5463=ORIENTED_EDGE('',*,*,#4164,.T.);
#5464=ORIENTED_EDGE('',*,*,#4167,.T.);
#5465=ORIENTED_EDGE('',*,*,#4170,.T.);
#5466=ORIENTED_EDGE('',*,*,#4173,.T.);
#5467=ORIENTED_EDGE('',*,*,#4176,.T.);
#5468=ORIENTED_EDGE('',*,*,#4179,.T.);
#5469=ORIENTED_EDGE('',*,*,#4181,.T.);
#5470=ORIENTED_EDGE('',*,*,#4183,.T.);
#5471=ORIENTED_EDGE('',*,*,#4185,.T.);
#5472=ORIENTED_EDGE('',*,*,#4187,.T.);
#5473=ORIENTED_EDGE('',*,*,#4189,.T.);
#5474=ORIENTED_EDGE('',*,*,#4191,.T.);
#5475=ORIENTED_EDGE('',*,*,#4193,.T.);
#5476=ORIENTED_EDGE('',*,*,#4195,.T.);
#5477=ORIENTED_EDGE('',*,*,#4156,.T.);
#5478=ORIENTED_EDGE('',*,*,#4198,.T.);
#5479=ORIENTED_EDGE('',*,*,#4159,.T.);
#5480=ORIENTED_EDGE('',*,*,#4199,.T.);
#5481=ORIENTED_EDGE('',*,*,#4162,.T.);
#5482=ORIENTED_EDGE('',*,*,#4200,.T.);
#5483=ORIENTED_EDGE('',*,*,#4165,.T.);
#5484=ORIENTED_EDGE('',*,*,#4201,.T.);
#5485=ORIENTED_EDGE('',*,*,#4168,.T.);
#5486=ORIENTED_EDGE('',*,*,#4202,.T.);
#5487=ORIENTED_EDGE('',*,*,#4171,.T.);
#5488=ORIENTED_EDGE('',*,*,#4203,.T.);
#5489=ORIENTED_EDGE('',*,*,#4174,.T.);
#5490=ORIENTED_EDGE('',*,*,#4204,.T.);
#5491=ORIENTED_EDGE('',*,*,#4177,.T.);
#5492=ORIENTED_EDGE('',*,*,#4205,.T.);
#5493=ORIENTED_EDGE('',*,*,#4206,.F.);
#5494=ORIENTED_EDGE('',*,*,#4207,.T.);
#5495=ORIENTED_EDGE('',*,*,#4208,.F.);
#5496=ORIENTED_EDGE('',*,*,#4209,.F.);
#5497=ORIENTED_EDGE('',*,*,#4210,.F.);
#5498=ORIENTED_EDGE('',*,*,#4209,.T.);
#5499=ORIENTED_EDGE('',*,*,#4211,.F.);
#5500=ORIENTED_EDGE('',*,*,#4212,.F.);
#5501=ORIENTED_EDGE('',*,*,#4213,.F.);
#5502=ORIENTED_EDGE('',*,*,#4212,.T.);
#5503=ORIENTED_EDGE('',*,*,#4214,.F.);
#5504=ORIENTED_EDGE('',*,*,#4215,.F.);
#5505=ORIENTED_EDGE('',*,*,#4216,.F.);
#5506=ORIENTED_EDGE('',*,*,#4215,.T.);
#5507=ORIENTED_EDGE('',*,*,#4217,.F.);
#5508=ORIENTED_EDGE('',*,*,#4218,.F.);
#5509=ORIENTED_EDGE('',*,*,#4219,.F.);
#5510=ORIENTED_EDGE('',*,*,#4218,.T.);
#5511=ORIENTED_EDGE('',*,*,#4220,.F.);
#5512=ORIENTED_EDGE('',*,*,#4221,.F.);
#5513=ORIENTED_EDGE('',*,*,#4222,.F.);
#5514=ORIENTED_EDGE('',*,*,#4221,.T.);
#5515=ORIENTED_EDGE('',*,*,#4223,.F.);
#5516=ORIENTED_EDGE('',*,*,#4224,.F.);
#5517=ORIENTED_EDGE('',*,*,#4225,.F.);
#5518=ORIENTED_EDGE('',*,*,#4224,.T.);
#5519=ORIENTED_EDGE('',*,*,#4226,.F.);
#5520=ORIENTED_EDGE('',*,*,#4227,.F.);
#5521=ORIENTED_EDGE('',*,*,#4228,.F.);
#5522=ORIENTED_EDGE('',*,*,#4227,.T.);
#5523=ORIENTED_EDGE('',*,*,#4229,.F.);
#5524=ORIENTED_EDGE('',*,*,#4230,.F.);
#5525=ORIENTED_EDGE('',*,*,#4231,.F.);
#5526=ORIENTED_EDGE('',*,*,#4230,.T.);
#5527=ORIENTED_EDGE('',*,*,#4140,.F.);
#5528=ORIENTED_EDGE('',*,*,#4232,.F.);
#5529=ORIENTED_EDGE('',*,*,#4233,.F.);
#5530=ORIENTED_EDGE('',*,*,#4232,.T.);
#5531=ORIENTED_EDGE('',*,*,#4139,.F.);
#5532=ORIENTED_EDGE('',*,*,#4234,.F.);
#5533=ORIENTED_EDGE('',*,*,#4235,.F.);
#5534=ORIENTED_EDGE('',*,*,#4234,.T.);
#5535=ORIENTED_EDGE('',*,*,#4138,.F.);
#5536=ORIENTED_EDGE('',*,*,#4236,.F.);
#5537=ORIENTED_EDGE('',*,*,#4237,.F.);
#5538=ORIENTED_EDGE('',*,*,#4236,.T.);
#5539=ORIENTED_EDGE('',*,*,#4137,.F.);
#5540=ORIENTED_EDGE('',*,*,#4238,.F.);
#5541=ORIENTED_EDGE('',*,*,#4239,.F.);
#5542=ORIENTED_EDGE('',*,*,#4238,.T.);
#5543=ORIENTED_EDGE('',*,*,#4136,.F.);
#5544=ORIENTED_EDGE('',*,*,#4240,.F.);
#5545=ORIENTED_EDGE('',*,*,#4241,.F.);
#5546=ORIENTED_EDGE('',*,*,#4240,.T.);
#5547=ORIENTED_EDGE('',*,*,#4135,.F.);
#5548=ORIENTED_EDGE('',*,*,#4242,.F.);
#5549=ORIENTED_EDGE('',*,*,#4243,.F.);
#5550=ORIENTED_EDGE('',*,*,#4242,.T.);
#5551=ORIENTED_EDGE('',*,*,#4134,.F.);
#5552=ORIENTED_EDGE('',*,*,#4244,.F.);
#5553=ORIENTED_EDGE('',*,*,#4245,.F.);
#5554=ORIENTED_EDGE('',*,*,#4244,.T.);
#5555=ORIENTED_EDGE('',*,*,#4133,.F.);
#5556=ORIENTED_EDGE('',*,*,#4246,.F.);
#5557=ORIENTED_EDGE('',*,*,#4247,.F.);
#5558=ORIENTED_EDGE('',*,*,#4246,.T.);
#5559=ORIENTED_EDGE('',*,*,#4132,.F.);
#5560=ORIENTED_EDGE('',*,*,#4248,.F.);
#5561=ORIENTED_EDGE('',*,*,#4249,.F.);
#5562=ORIENTED_EDGE('',*,*,#4248,.T.);
#5563=ORIENTED_EDGE('',*,*,#4131,.F.);
#5564=ORIENTED_EDGE('',*,*,#4207,.F.);
#5565=ORIENTED_EDGE('',*,*,#4249,.T.);
#5566=ORIENTED_EDGE('',*,*,#4206,.T.);
#5567=ORIENTED_EDGE('',*,*,#4210,.T.);
#5568=ORIENTED_EDGE('',*,*,#4213,.T.);
#5569=ORIENTED_EDGE('',*,*,#4216,.T.);
#5570=ORIENTED_EDGE('',*,*,#4219,.T.);
#5571=ORIENTED_EDGE('',*,*,#4222,.T.);
#5572=ORIENTED_EDGE('',*,*,#4225,.T.);
#5573=ORIENTED_EDGE('',*,*,#4228,.T.);
#5574=ORIENTED_EDGE('',*,*,#4231,.T.);
#5575=ORIENTED_EDGE('',*,*,#4233,.T.);
#5576=ORIENTED_EDGE('',*,*,#4235,.T.);
#5577=ORIENTED_EDGE('',*,*,#4237,.T.);
#5578=ORIENTED_EDGE('',*,*,#4239,.T.);
#5579=ORIENTED_EDGE('',*,*,#4241,.T.);
#5580=ORIENTED_EDGE('',*,*,#4243,.T.);
#5581=ORIENTED_EDGE('',*,*,#4245,.T.);
#5582=ORIENTED_EDGE('',*,*,#4247,.T.);
#5583=ORIENTED_EDGE('',*,*,#4208,.T.);
#5584=ORIENTED_EDGE('',*,*,#4250,.T.);
#5585=ORIENTED_EDGE('',*,*,#4211,.T.);
#5586=ORIENTED_EDGE('',*,*,#4251,.T.);
#5587=ORIENTED_EDGE('',*,*,#4214,.T.);
#5588=ORIENTED_EDGE('',*,*,#4252,.T.);
#5589=ORIENTED_EDGE('',*,*,#4217,.T.);
#5590=ORIENTED_EDGE('',*,*,#4253,.T.);
#5591=ORIENTED_EDGE('',*,*,#4220,.T.);
#5592=ORIENTED_EDGE('',*,*,#4254,.T.);
#5593=ORIENTED_EDGE('',*,*,#4223,.T.);
#5594=ORIENTED_EDGE('',*,*,#4255,.T.);
#5595=ORIENTED_EDGE('',*,*,#4226,.T.);
#5596=ORIENTED_EDGE('',*,*,#4256,.T.);
#5597=ORIENTED_EDGE('',*,*,#4229,.T.);
#5598=ORIENTED_EDGE('',*,*,#4257,.T.);
#5599=ORIENTED_EDGE('',*,*,#4258,.F.);
#5600=ORIENTED_EDGE('',*,*,#4259,.T.);
#5601=ORIENTED_EDGE('',*,*,#4152,.F.);
#5602=ORIENTED_EDGE('',*,*,#4205,.F.);
#5603=ORIENTED_EDGE('',*,*,#4204,.F.);
#5604=ORIENTED_EDGE('',*,*,#4203,.F.);
#5605=ORIENTED_EDGE('',*,*,#4202,.F.);
#5606=ORIENTED_EDGE('',*,*,#4201,.F.);
#5607=ORIENTED_EDGE('',*,*,#4200,.F.);
#5608=ORIENTED_EDGE('',*,*,#4199,.F.);
#5609=ORIENTED_EDGE('',*,*,#4198,.F.);
#5610=ORIENTED_EDGE('',*,*,#4141,.F.);
#5611=ORIENTED_EDGE('',*,*,#4257,.F.);
#5612=ORIENTED_EDGE('',*,*,#4256,.F.);
#5613=ORIENTED_EDGE('',*,*,#4255,.F.);
#5614=ORIENTED_EDGE('',*,*,#4254,.F.);
#5615=ORIENTED_EDGE('',*,*,#4253,.F.);
#5616=ORIENTED_EDGE('',*,*,#4252,.F.);
#5617=ORIENTED_EDGE('',*,*,#4251,.F.);
#5618=ORIENTED_EDGE('',*,*,#4250,.F.);
#5619=ORIENTED_EDGE('',*,*,#4130,.F.);
#5620=ORIENTED_EDGE('',*,*,#4129,.F.);
#5621=ORIENTED_EDGE('',*,*,#4128,.F.);
#5622=ORIENTED_EDGE('',*,*,#4127,.F.);
#5623=ORIENTED_EDGE('',*,*,#4126,.F.);
#5624=ORIENTED_EDGE('',*,*,#4125,.F.);
#5625=ORIENTED_EDGE('',*,*,#4124,.F.);
#5626=ORIENTED_EDGE('',*,*,#4123,.F.);
#5627=ORIENTED_EDGE('',*,*,#4122,.F.);
#5628=ORIENTED_EDGE('',*,*,#4153,.F.);
#5629=ORIENTED_EDGE('',*,*,#4259,.F.);
#5630=ORIENTED_EDGE('',*,*,#4064,.T.);
#5631=ORIENTED_EDGE('',*,*,#4258,.T.);
#5632=ORIENTED_EDGE('',*,*,#4065,.T.);
#5633=ORIENTED_EDGE('',*,*,#4260,.F.);
#5634=ORIENTED_EDGE('',*,*,#4261,.F.);
#5635=ORIENTED_EDGE('',*,*,#4262,.T.);
#5636=ORIENTED_EDGE('',*,*,#4263,.F.);
#5637=ORIENTED_EDGE('',*,*,#4264,.F.);
#5638=ORIENTED_EDGE('',*,*,#4262,.F.);
#5639=ORIENTED_EDGE('',*,*,#4265,.F.);
#5640=ORIENTED_EDGE('',*,*,#4266,.T.);
#5641=ORIENTED_EDGE('',*,*,#4267,.F.);
#5642=ORIENTED_EDGE('',*,*,#4266,.F.);
#5643=ORIENTED_EDGE('',*,*,#4260,.T.);
#5644=ORIENTED_EDGE('',*,*,#4261,.T.);
#5645=ORIENTED_EDGE('',*,*,#4268,.T.);
#5646=ORIENTED_EDGE('',*,*,#4269,.T.);
#5647=ORIENTED_EDGE('',*,*,#4270,.F.);
#5648=ORIENTED_EDGE('',*,*,#4271,.F.);
#5649=ORIENTED_EDGE('',*,*,#4272,.T.);
#5650=ORIENTED_EDGE('',*,*,#4271,.T.);
#5651=ORIENTED_EDGE('',*,*,#4273,.F.);
#5652=ORIENTED_EDGE('',*,*,#4274,.F.);
#5653=ORIENTED_EDGE('',*,*,#4275,.T.);
#5654=ORIENTED_EDGE('',*,*,#4274,.T.);
#5655=ORIENTED_EDGE('',*,*,#4276,.F.);
#5656=ORIENTED_EDGE('',*,*,#4277,.F.);
#5657=ORIENTED_EDGE('',*,*,#4278,.T.);
#5658=ORIENTED_EDGE('',*,*,#4277,.T.);
#5659=ORIENTED_EDGE('',*,*,#4279,.F.);
#5660=ORIENTED_EDGE('',*,*,#4280,.F.);
#5661=ORIENTED_EDGE('',*,*,#4281,.T.);
#5662=ORIENTED_EDGE('',*,*,#4280,.T.);
#5663=ORIENTED_EDGE('',*,*,#4282,.F.);
#5664=ORIENTED_EDGE('',*,*,#4283,.F.);
#5665=ORIENTED_EDGE('',*,*,#4284,.T.);
#5666=ORIENTED_EDGE('',*,*,#4283,.T.);
#5667=ORIENTED_EDGE('',*,*,#4285,.F.);
#5668=ORIENTED_EDGE('',*,*,#4286,.F.);
#5669=ORIENTED_EDGE('',*,*,#4287,.T.);
#5670=ORIENTED_EDGE('',*,*,#4286,.T.);
#5671=ORIENTED_EDGE('',*,*,#4288,.F.);
#5672=ORIENTED_EDGE('',*,*,#4289,.F.);
#5673=ORIENTED_EDGE('',*,*,#4290,.T.);
#5674=ORIENTED_EDGE('',*,*,#4289,.T.);
#5675=ORIENTED_EDGE('',*,*,#4291,.F.);
#5676=ORIENTED_EDGE('',*,*,#4292,.F.);
#5677=ORIENTED_EDGE('',*,*,#4293,.T.);
#5678=ORIENTED_EDGE('',*,*,#4292,.T.);
#5679=ORIENTED_EDGE('',*,*,#4294,.F.);
#5680=ORIENTED_EDGE('',*,*,#4295,.F.);
#5681=ORIENTED_EDGE('',*,*,#4296,.T.);
#5682=ORIENTED_EDGE('',*,*,#4295,.T.);
#5683=ORIENTED_EDGE('',*,*,#4297,.F.);
#5684=ORIENTED_EDGE('',*,*,#4298,.F.);
#5685=ORIENTED_EDGE('',*,*,#4299,.T.);
#5686=ORIENTED_EDGE('',*,*,#4298,.T.);
#5687=ORIENTED_EDGE('',*,*,#4300,.F.);
#5688=ORIENTED_EDGE('',*,*,#4301,.F.);
#5689=ORIENTED_EDGE('',*,*,#4302,.T.);
#5690=ORIENTED_EDGE('',*,*,#4301,.T.);
#5691=ORIENTED_EDGE('',*,*,#4303,.F.);
#5692=ORIENTED_EDGE('',*,*,#4304,.F.);
#5693=ORIENTED_EDGE('',*,*,#4305,.T.);
#5694=ORIENTED_EDGE('',*,*,#4304,.T.);
#5695=ORIENTED_EDGE('',*,*,#4306,.F.);
#5696=ORIENTED_EDGE('',*,*,#4307,.F.);
#5697=ORIENTED_EDGE('',*,*,#4308,.T.);
#5698=ORIENTED_EDGE('',*,*,#4307,.T.);
#5699=ORIENTED_EDGE('',*,*,#4309,.F.);
#5700=ORIENTED_EDGE('',*,*,#4310,.F.);
#5701=ORIENTED_EDGE('',*,*,#4311,.T.);
#5702=ORIENTED_EDGE('',*,*,#4310,.T.);
#5703=ORIENTED_EDGE('',*,*,#4312,.F.);
#5704=ORIENTED_EDGE('',*,*,#4313,.F.);
#5705=ORIENTED_EDGE('',*,*,#4314,.T.);
#5706=ORIENTED_EDGE('',*,*,#4313,.T.);
#5707=ORIENTED_EDGE('',*,*,#4315,.F.);
#5708=ORIENTED_EDGE('',*,*,#4316,.F.);
#5709=ORIENTED_EDGE('',*,*,#4317,.T.);
#5710=ORIENTED_EDGE('',*,*,#4316,.T.);
#5711=ORIENTED_EDGE('',*,*,#4318,.F.);
#5712=ORIENTED_EDGE('',*,*,#4319,.F.);
#5713=ORIENTED_EDGE('',*,*,#4320,.T.);
#5714=ORIENTED_EDGE('',*,*,#4319,.T.);
#5715=ORIENTED_EDGE('',*,*,#4321,.F.);
#5716=ORIENTED_EDGE('',*,*,#4269,.F.);
#5717=ORIENTED_EDGE('',*,*,#4320,.F.);
#5718=ORIENTED_EDGE('',*,*,#4268,.F.);
#5719=ORIENTED_EDGE('',*,*,#4272,.F.);
#5720=ORIENTED_EDGE('',*,*,#4275,.F.);
#5721=ORIENTED_EDGE('',*,*,#4278,.F.);
#5722=ORIENTED_EDGE('',*,*,#4281,.F.);
#5723=ORIENTED_EDGE('',*,*,#4284,.F.);
#5724=ORIENTED_EDGE('',*,*,#4287,.F.);
#5725=ORIENTED_EDGE('',*,*,#4290,.F.);
#5726=ORIENTED_EDGE('',*,*,#4293,.F.);
#5727=ORIENTED_EDGE('',*,*,#4296,.F.);
#5728=ORIENTED_EDGE('',*,*,#4299,.F.);
#5729=ORIENTED_EDGE('',*,*,#4302,.F.);
#5730=ORIENTED_EDGE('',*,*,#4305,.F.);
#5731=ORIENTED_EDGE('',*,*,#4308,.F.);
#5732=ORIENTED_EDGE('',*,*,#4311,.F.);
#5733=ORIENTED_EDGE('',*,*,#4314,.F.);
#5734=ORIENTED_EDGE('',*,*,#4317,.F.);
#5735=ORIENTED_EDGE('',*,*,#4318,.T.);
#5736=ORIENTED_EDGE('',*,*,#4322,.F.);
#5737=ORIENTED_EDGE('',*,*,#4315,.T.);
#5738=ORIENTED_EDGE('',*,*,#4323,.F.);
#5739=ORIENTED_EDGE('',*,*,#4312,.T.);
#5740=ORIENTED_EDGE('',*,*,#4324,.F.);
#5741=ORIENTED_EDGE('',*,*,#4309,.T.);
#5742=ORIENTED_EDGE('',*,*,#4325,.F.);
#5743=ORIENTED_EDGE('',*,*,#4306,.T.);
#5744=ORIENTED_EDGE('',*,*,#4326,.F.);
#5745=ORIENTED_EDGE('',*,*,#4303,.T.);
#5746=ORIENTED_EDGE('',*,*,#4327,.F.);
#5747=ORIENTED_EDGE('',*,*,#4294,.T.);
#5748=ORIENTED_EDGE('',*,*,#4291,.T.);
#5749=ORIENTED_EDGE('',*,*,#4288,.T.);
#5750=ORIENTED_EDGE('',*,*,#4285,.T.);
#5751=ORIENTED_EDGE('',*,*,#4282,.T.);
#5752=ORIENTED_EDGE('',*,*,#4279,.T.);
#5753=ORIENTED_EDGE('',*,*,#4276,.T.);
#5754=ORIENTED_EDGE('',*,*,#4273,.T.);
#5755=ORIENTED_EDGE('',*,*,#4270,.T.);
#5756=ORIENTED_EDGE('',*,*,#4321,.T.);
#5757=ORIENTED_EDGE('',*,*,#4328,.F.);
#5758=ORIENTED_EDGE('',*,*,#4329,.F.);
#5759=ORIENTED_EDGE('',*,*,#4330,.T.);
#5760=ORIENTED_EDGE('',*,*,#4331,.T.);
#5761=ORIENTED_EDGE('',*,*,#4332,.T.);
#5762=ORIENTED_EDGE('',*,*,#4333,.T.);
#5763=ORIENTED_EDGE('',*,*,#4334,.T.);
#5764=ORIENTED_EDGE('',*,*,#4335,.T.);
#5765=ORIENTED_EDGE('',*,*,#4336,.T.);
#5766=ORIENTED_EDGE('',*,*,#4337,.T.);
#5767=ORIENTED_EDGE('',*,*,#4338,.T.);
#5768=ORIENTED_EDGE('',*,*,#4339,.T.);
#5769=ORIENTED_EDGE('',*,*,#4340,.F.);
#5770=ORIENTED_EDGE('',*,*,#4341,.T.);
#5771=ORIENTED_EDGE('',*,*,#4342,.T.);
#5772=ORIENTED_EDGE('',*,*,#4343,.T.);
#5773=ORIENTED_EDGE('',*,*,#4344,.T.);
#5774=ORIENTED_EDGE('',*,*,#4345,.T.);
#5775=ORIENTED_EDGE('',*,*,#4346,.T.);
#5776=ORIENTED_EDGE('',*,*,#4347,.T.);
#5777=ORIENTED_EDGE('',*,*,#4348,.T.);
#5778=ORIENTED_EDGE('',*,*,#4349,.T.);
#5779=ORIENTED_EDGE('',*,*,#4350,.T.);
#5780=ORIENTED_EDGE('',*,*,#4351,.F.);
#5781=ORIENTED_EDGE('',*,*,#4265,.T.);
#5782=ORIENTED_EDGE('',*,*,#4297,.T.);
#5783=ORIENTED_EDGE('',*,*,#4352,.F.);
#5784=ORIENTED_EDGE('',*,*,#4300,.T.);
#5785=ORIENTED_EDGE('',*,*,#4353,.F.);
#5786=ORIENTED_EDGE('',*,*,#4354,.T.);
#5787=ORIENTED_EDGE('',*,*,#4355,.T.);
#5788=ORIENTED_EDGE('',*,*,#4338,.F.);
#5789=ORIENTED_EDGE('',*,*,#4356,.F.);
#5790=ORIENTED_EDGE('',*,*,#4357,.T.);
#5791=ORIENTED_EDGE('',*,*,#4356,.T.);
#5792=ORIENTED_EDGE('',*,*,#4337,.F.);
#5793=ORIENTED_EDGE('',*,*,#4358,.F.);
#5794=ORIENTED_EDGE('',*,*,#4359,.T.);
#5795=ORIENTED_EDGE('',*,*,#4358,.T.);
#5796=ORIENTED_EDGE('',*,*,#4336,.F.);
#5797=ORIENTED_EDGE('',*,*,#4360,.F.);
#5798=ORIENTED_EDGE('',*,*,#4361,.T.);
#5799=ORIENTED_EDGE('',*,*,#4360,.T.);
#5800=ORIENTED_EDGE('',*,*,#4335,.F.);
#5801=ORIENTED_EDGE('',*,*,#4362,.F.);
#5802=ORIENTED_EDGE('',*,*,#4363,.T.);
#5803=ORIENTED_EDGE('',*,*,#4362,.T.);
#5804=ORIENTED_EDGE('',*,*,#4334,.F.);
#5805=ORIENTED_EDGE('',*,*,#4364,.F.);
#5806=ORIENTED_EDGE('',*,*,#4365,.T.);
#5807=ORIENTED_EDGE('',*,*,#4364,.T.);
#5808=ORIENTED_EDGE('',*,*,#4333,.F.);
#5809=ORIENTED_EDGE('',*,*,#4366,.F.);
#5810=ORIENTED_EDGE('',*,*,#4367,.T.);
#5811=ORIENTED_EDGE('',*,*,#4366,.T.);
#5812=ORIENTED_EDGE('',*,*,#4332,.F.);
#5813=ORIENTED_EDGE('',*,*,#4368,.F.);
#5814=ORIENTED_EDGE('',*,*,#4369,.T.);
#5815=ORIENTED_EDGE('',*,*,#4368,.T.);
#5816=ORIENTED_EDGE('',*,*,#4331,.F.);
#5817=ORIENTED_EDGE('',*,*,#4370,.F.);
#5818=ORIENTED_EDGE('',*,*,#4371,.T.);
#5819=ORIENTED_EDGE('',*,*,#4370,.T.);
#5820=ORIENTED_EDGE('',*,*,#4330,.F.);
#5821=ORIENTED_EDGE('',*,*,#4372,.F.);
#5822=ORIENTED_EDGE('',*,*,#4373,.T.);
#5823=ORIENTED_EDGE('',*,*,#4372,.T.);
#5824=ORIENTED_EDGE('',*,*,#4374,.F.);
#5825=ORIENTED_EDGE('',*,*,#4375,.F.);
#5826=ORIENTED_EDGE('',*,*,#4376,.T.);
#5827=ORIENTED_EDGE('',*,*,#4375,.T.);
#5828=ORIENTED_EDGE('',*,*,#4377,.F.);
#5829=ORIENTED_EDGE('',*,*,#4378,.F.);
#5830=ORIENTED_EDGE('',*,*,#4379,.T.);
#5831=ORIENTED_EDGE('',*,*,#4378,.T.);
#5832=ORIENTED_EDGE('',*,*,#4380,.F.);
#5833=ORIENTED_EDGE('',*,*,#4381,.F.);
#5834=ORIENTED_EDGE('',*,*,#4382,.T.);
#5835=ORIENTED_EDGE('',*,*,#4381,.T.);
#5836=ORIENTED_EDGE('',*,*,#4383,.F.);
#5837=ORIENTED_EDGE('',*,*,#4384,.F.);
#5838=ORIENTED_EDGE('',*,*,#4385,.T.);
#5839=ORIENTED_EDGE('',*,*,#4384,.T.);
#5840=ORIENTED_EDGE('',*,*,#4386,.F.);
#5841=ORIENTED_EDGE('',*,*,#4387,.F.);
#5842=ORIENTED_EDGE('',*,*,#4388,.T.);
#5843=ORIENTED_EDGE('',*,*,#4387,.T.);
#5844=ORIENTED_EDGE('',*,*,#4389,.F.);
#5845=ORIENTED_EDGE('',*,*,#4390,.F.);
#5846=ORIENTED_EDGE('',*,*,#4391,.T.);
#5847=ORIENTED_EDGE('',*,*,#4390,.T.);
#5848=ORIENTED_EDGE('',*,*,#4392,.F.);
#5849=ORIENTED_EDGE('',*,*,#4393,.F.);
#5850=ORIENTED_EDGE('',*,*,#4394,.T.);
#5851=ORIENTED_EDGE('',*,*,#4393,.T.);
#5852=ORIENTED_EDGE('',*,*,#4395,.F.);
#5853=ORIENTED_EDGE('',*,*,#4396,.F.);
#5854=ORIENTED_EDGE('',*,*,#4397,.T.);
#5855=ORIENTED_EDGE('',*,*,#4396,.T.);
#5856=ORIENTED_EDGE('',*,*,#4339,.F.);
#5857=ORIENTED_EDGE('',*,*,#4355,.F.);
#5858=ORIENTED_EDGE('',*,*,#4397,.F.);
#5859=ORIENTED_EDGE('',*,*,#4354,.F.);
#5860=ORIENTED_EDGE('',*,*,#4357,.F.);
#5861=ORIENTED_EDGE('',*,*,#4359,.F.);
#5862=ORIENTED_EDGE('',*,*,#4361,.F.);
#5863=ORIENTED_EDGE('',*,*,#4363,.F.);
#5864=ORIENTED_EDGE('',*,*,#4365,.F.);
#5865=ORIENTED_EDGE('',*,*,#4367,.F.);
#5866=ORIENTED_EDGE('',*,*,#4369,.F.);
#5867=ORIENTED_EDGE('',*,*,#4371,.F.);
#5868=ORIENTED_EDGE('',*,*,#4373,.F.);
#5869=ORIENTED_EDGE('',*,*,#4376,.F.);
#5870=ORIENTED_EDGE('',*,*,#4379,.F.);
#5871=ORIENTED_EDGE('',*,*,#4382,.F.);
#5872=ORIENTED_EDGE('',*,*,#4385,.F.);
#5873=ORIENTED_EDGE('',*,*,#4388,.F.);
#5874=ORIENTED_EDGE('',*,*,#4391,.F.);
#5875=ORIENTED_EDGE('',*,*,#4394,.F.);
#5876=ORIENTED_EDGE('',*,*,#4395,.T.);
#5877=ORIENTED_EDGE('',*,*,#4398,.F.);
#5878=ORIENTED_EDGE('',*,*,#4392,.T.);
#5879=ORIENTED_EDGE('',*,*,#4399,.F.);
#5880=ORIENTED_EDGE('',*,*,#4389,.T.);
#5881=ORIENTED_EDGE('',*,*,#4400,.F.);
#5882=ORIENTED_EDGE('',*,*,#4386,.T.);
#5883=ORIENTED_EDGE('',*,*,#4401,.F.);
#5884=ORIENTED_EDGE('',*,*,#4383,.T.);
#5885=ORIENTED_EDGE('',*,*,#4402,.F.);
#5886=ORIENTED_EDGE('',*,*,#4380,.T.);
#5887=ORIENTED_EDGE('',*,*,#4403,.F.);
#5888=ORIENTED_EDGE('',*,*,#4374,.T.);
#5889=ORIENTED_EDGE('',*,*,#4404,.F.);
#5890=ORIENTED_EDGE('',*,*,#4377,.T.);
#5891=ORIENTED_EDGE('',*,*,#4405,.F.);
#5892=ORIENTED_EDGE('',*,*,#4406,.T.);
#5893=ORIENTED_EDGE('',*,*,#4407,.T.);
#5894=ORIENTED_EDGE('',*,*,#4349,.F.);
#5895=ORIENTED_EDGE('',*,*,#4408,.F.);
#5896=ORIENTED_EDGE('',*,*,#4409,.T.);
#5897=ORIENTED_EDGE('',*,*,#4408,.T.);
#5898=ORIENTED_EDGE('',*,*,#4348,.F.);
#5899=ORIENTED_EDGE('',*,*,#4410,.F.);
#5900=ORIENTED_EDGE('',*,*,#4411,.T.);
#5901=ORIENTED_EDGE('',*,*,#4410,.T.);
#5902=ORIENTED_EDGE('',*,*,#4347,.F.);
#5903=ORIENTED_EDGE('',*,*,#4412,.F.);
#5904=ORIENTED_EDGE('',*,*,#4413,.T.);
#5905=ORIENTED_EDGE('',*,*,#4412,.T.);
#5906=ORIENTED_EDGE('',*,*,#4346,.F.);
#5907=ORIENTED_EDGE('',*,*,#4414,.F.);
#5908=ORIENTED_EDGE('',*,*,#4415,.T.);
#5909=ORIENTED_EDGE('',*,*,#4414,.T.);
#5910=ORIENTED_EDGE('',*,*,#4345,.F.);
#5911=ORIENTED_EDGE('',*,*,#4416,.F.);
#5912=ORIENTED_EDGE('',*,*,#4417,.T.);
#5913=ORIENTED_EDGE('',*,*,#4416,.T.);
#5914=ORIENTED_EDGE('',*,*,#4344,.F.);
#5915=ORIENTED_EDGE('',*,*,#4418,.F.);
#5916=ORIENTED_EDGE('',*,*,#4419,.T.);
#5917=ORIENTED_EDGE('',*,*,#4418,.T.);
#5918=ORIENTED_EDGE('',*,*,#4343,.F.);
#5919=ORIENTED_EDGE('',*,*,#4420,.F.);
#5920=ORIENTED_EDGE('',*,*,#4421,.T.);
#5921=ORIENTED_EDGE('',*,*,#4420,.T.);
#5922=ORIENTED_EDGE('',*,*,#4342,.F.);
#5923=ORIENTED_EDGE('',*,*,#4422,.F.);
#5924=ORIENTED_EDGE('',*,*,#4423,.T.);
#5925=ORIENTED_EDGE('',*,*,#4422,.T.);
#5926=ORIENTED_EDGE('',*,*,#4341,.F.);
#5927=ORIENTED_EDGE('',*,*,#4424,.F.);
#5928=ORIENTED_EDGE('',*,*,#4425,.T.);
#5929=ORIENTED_EDGE('',*,*,#4424,.T.);
#5930=ORIENTED_EDGE('',*,*,#4426,.F.);
#5931=ORIENTED_EDGE('',*,*,#4427,.F.);
#5932=ORIENTED_EDGE('',*,*,#4428,.T.);
#5933=ORIENTED_EDGE('',*,*,#4427,.T.);
#5934=ORIENTED_EDGE('',*,*,#4429,.F.);
#5935=ORIENTED_EDGE('',*,*,#4430,.F.);
#5936=ORIENTED_EDGE('',*,*,#4431,.T.);
#5937=ORIENTED_EDGE('',*,*,#4430,.T.);
#5938=ORIENTED_EDGE('',*,*,#4432,.F.);
#5939=ORIENTED_EDGE('',*,*,#4433,.F.);
#5940=ORIENTED_EDGE('',*,*,#4434,.T.);
#5941=ORIENTED_EDGE('',*,*,#4433,.T.);
#5942=ORIENTED_EDGE('',*,*,#4435,.F.);
#5943=ORIENTED_EDGE('',*,*,#4436,.F.);
#5944=ORIENTED_EDGE('',*,*,#4437,.T.);
#5945=ORIENTED_EDGE('',*,*,#4436,.T.);
#5946=ORIENTED_EDGE('',*,*,#4438,.F.);
#5947=ORIENTED_EDGE('',*,*,#4439,.F.);
#5948=ORIENTED_EDGE('',*,*,#4440,.T.);
#5949=ORIENTED_EDGE('',*,*,#4439,.T.);
#5950=ORIENTED_EDGE('',*,*,#4441,.F.);
#5951=ORIENTED_EDGE('',*,*,#4442,.F.);
#5952=ORIENTED_EDGE('',*,*,#4443,.T.);
#5953=ORIENTED_EDGE('',*,*,#4442,.T.);
#5954=ORIENTED_EDGE('',*,*,#4444,.F.);
#5955=ORIENTED_EDGE('',*,*,#4445,.F.);
#5956=ORIENTED_EDGE('',*,*,#4446,.T.);
#5957=ORIENTED_EDGE('',*,*,#4445,.T.);
#5958=ORIENTED_EDGE('',*,*,#4447,.F.);
#5959=ORIENTED_EDGE('',*,*,#4448,.F.);
#5960=ORIENTED_EDGE('',*,*,#4449,.T.);
#5961=ORIENTED_EDGE('',*,*,#4448,.T.);
#5962=ORIENTED_EDGE('',*,*,#4350,.F.);
#5963=ORIENTED_EDGE('',*,*,#4407,.F.);
#5964=ORIENTED_EDGE('',*,*,#4449,.F.);
#5965=ORIENTED_EDGE('',*,*,#4406,.F.);
#5966=ORIENTED_EDGE('',*,*,#4409,.F.);
#5967=ORIENTED_EDGE('',*,*,#4411,.F.);
#5968=ORIENTED_EDGE('',*,*,#4413,.F.);
#5969=ORIENTED_EDGE('',*,*,#4415,.F.);
#5970=ORIENTED_EDGE('',*,*,#4417,.F.);
#5971=ORIENTED_EDGE('',*,*,#4419,.F.);
#5972=ORIENTED_EDGE('',*,*,#4421,.F.);
#5973=ORIENTED_EDGE('',*,*,#4423,.F.);
#5974=ORIENTED_EDGE('',*,*,#4425,.F.);
#5975=ORIENTED_EDGE('',*,*,#4428,.F.);
#5976=ORIENTED_EDGE('',*,*,#4431,.F.);
#5977=ORIENTED_EDGE('',*,*,#4434,.F.);
#5978=ORIENTED_EDGE('',*,*,#4437,.F.);
#5979=ORIENTED_EDGE('',*,*,#4440,.F.);
#5980=ORIENTED_EDGE('',*,*,#4443,.F.);
#5981=ORIENTED_EDGE('',*,*,#4446,.F.);
#5982=ORIENTED_EDGE('',*,*,#4447,.T.);
#5983=ORIENTED_EDGE('',*,*,#4450,.F.);
#5984=ORIENTED_EDGE('',*,*,#4444,.T.);
#5985=ORIENTED_EDGE('',*,*,#4451,.F.);
#5986=ORIENTED_EDGE('',*,*,#4441,.T.);
#5987=ORIENTED_EDGE('',*,*,#4452,.F.);
#5988=ORIENTED_EDGE('',*,*,#4438,.T.);
#5989=ORIENTED_EDGE('',*,*,#4453,.F.);
#5990=ORIENTED_EDGE('',*,*,#4435,.T.);
#5991=ORIENTED_EDGE('',*,*,#4454,.F.);
#5992=ORIENTED_EDGE('',*,*,#4432,.T.);
#5993=ORIENTED_EDGE('',*,*,#4455,.F.);
#5994=ORIENTED_EDGE('',*,*,#4426,.T.);
#5995=ORIENTED_EDGE('',*,*,#4456,.F.);
#5996=ORIENTED_EDGE('',*,*,#4429,.T.);
#5997=ORIENTED_EDGE('',*,*,#4457,.F.);
#5998=ORIENTED_EDGE('',*,*,#4458,.F.);
#5999=ORIENTED_EDGE('',*,*,#4459,.T.);
#6000=ORIENTED_EDGE('',*,*,#4328,.T.);
#6001=ORIENTED_EDGE('',*,*,#4322,.T.);
#6002=ORIENTED_EDGE('',*,*,#4323,.T.);
#6003=ORIENTED_EDGE('',*,*,#4324,.T.);
#6004=ORIENTED_EDGE('',*,*,#4325,.T.);
#6005=ORIENTED_EDGE('',*,*,#4326,.T.);
#6006=ORIENTED_EDGE('',*,*,#4327,.T.);
#6007=ORIENTED_EDGE('',*,*,#4353,.T.);
#6008=ORIENTED_EDGE('',*,*,#4352,.T.);
#6009=ORIENTED_EDGE('',*,*,#4351,.T.);
#6010=ORIENTED_EDGE('',*,*,#4450,.T.);
#6011=ORIENTED_EDGE('',*,*,#4451,.T.);
#6012=ORIENTED_EDGE('',*,*,#4452,.T.);
#6013=ORIENTED_EDGE('',*,*,#4453,.T.);
#6014=ORIENTED_EDGE('',*,*,#4454,.T.);
#6015=ORIENTED_EDGE('',*,*,#4455,.T.);
#6016=ORIENTED_EDGE('',*,*,#4457,.T.);
#6017=ORIENTED_EDGE('',*,*,#4456,.T.);
#6018=ORIENTED_EDGE('',*,*,#4340,.T.);
#6019=ORIENTED_EDGE('',*,*,#4398,.T.);
#6020=ORIENTED_EDGE('',*,*,#4399,.T.);
#6021=ORIENTED_EDGE('',*,*,#4400,.T.);
#6022=ORIENTED_EDGE('',*,*,#4401,.T.);
#6023=ORIENTED_EDGE('',*,*,#4402,.T.);
#6024=ORIENTED_EDGE('',*,*,#4403,.T.);
#6025=ORIENTED_EDGE('',*,*,#4405,.T.);
#6026=ORIENTED_EDGE('',*,*,#4404,.T.);
#6027=ORIENTED_EDGE('',*,*,#4329,.T.);
#6028=ORIENTED_EDGE('',*,*,#4459,.F.);
#6029=ORIENTED_EDGE('',*,*,#4263,.T.);
#6030=ORIENTED_EDGE('',*,*,#4264,.T.);
#6031=ORIENTED_EDGE('',*,*,#4458,.T.);
#6032=ORIENTED_EDGE('',*,*,#4267,.T.);
#6033=ORIENTED_EDGE('',*,*,#4460,.F.);
#6034=ORIENTED_EDGE('',*,*,#4461,.F.);
#6035=ORIENTED_EDGE('',*,*,#4462,.F.);
#6036=ORIENTED_EDGE('',*,*,#4463,.F.);
#6037=ORIENTED_EDGE('',*,*,#4464,.F.);
#6038=ORIENTED_EDGE('',*,*,#4465,.F.);
#6039=ORIENTED_EDGE('',*,*,#4466,.F.);
#6040=ORIENTED_EDGE('',*,*,#4467,.F.);
#6041=ORIENTED_EDGE('',*,*,#4468,.T.);
#6042=ORIENTED_EDGE('',*,*,#4469,.F.);
#6043=ORIENTED_EDGE('',*,*,#4470,.F.);
#6044=ORIENTED_EDGE('',*,*,#4471,.F.);
#6045=ORIENTED_EDGE('',*,*,#4472,.F.);
#6046=ORIENTED_EDGE('',*,*,#4473,.F.);
#6047=ORIENTED_EDGE('',*,*,#4474,.F.);
#6048=ORIENTED_EDGE('',*,*,#4475,.F.);
#6049=ORIENTED_EDGE('',*,*,#4476,.F.);
#6050=ORIENTED_EDGE('',*,*,#4477,.T.);
#6051=ORIENTED_EDGE('',*,*,#4478,.F.);
#6052=ORIENTED_EDGE('',*,*,#4479,.F.);
#6053=ORIENTED_EDGE('',*,*,#4480,.F.);
#6054=ORIENTED_EDGE('',*,*,#4481,.F.);
#6055=ORIENTED_EDGE('',*,*,#4482,.F.);
#6056=ORIENTED_EDGE('',*,*,#4483,.F.);
#6057=ORIENTED_EDGE('',*,*,#4484,.F.);
#6058=ORIENTED_EDGE('',*,*,#4485,.F.);
#6059=ORIENTED_EDGE('',*,*,#4486,.T.);
#6060=ORIENTED_EDGE('',*,*,#4487,.F.);
#6061=ORIENTED_EDGE('',*,*,#4488,.F.);
#6062=ORIENTED_EDGE('',*,*,#4489,.F.);
#6063=ORIENTED_EDGE('',*,*,#4490,.F.);
#6064=ORIENTED_EDGE('',*,*,#4491,.F.);
#6065=ORIENTED_EDGE('',*,*,#4492,.F.);
#6066=ORIENTED_EDGE('',*,*,#4493,.F.);
#6067=ORIENTED_EDGE('',*,*,#4494,.F.);
#6068=ORIENTED_EDGE('',*,*,#4495,.T.);
#6069=ORIENTED_EDGE('',*,*,#4496,.F.);
#6070=ORIENTED_EDGE('',*,*,#4497,.F.);
#6071=ORIENTED_EDGE('',*,*,#4498,.F.);
#6072=ORIENTED_EDGE('',*,*,#4499,.F.);
#6073=ORIENTED_EDGE('',*,*,#4500,.F.);
#6074=ORIENTED_EDGE('',*,*,#4501,.F.);
#6075=ORIENTED_EDGE('',*,*,#4502,.F.);
#6076=ORIENTED_EDGE('',*,*,#4503,.F.);
#6077=ORIENTED_EDGE('',*,*,#4504,.T.);
#6078=ORIENTED_EDGE('',*,*,#4505,.F.);
#6079=ORIENTED_EDGE('',*,*,#4506,.F.);
#6080=ORIENTED_EDGE('',*,*,#4507,.F.);
#6081=ORIENTED_EDGE('',*,*,#4508,.F.);
#6082=ORIENTED_EDGE('',*,*,#4509,.F.);
#6083=ORIENTED_EDGE('',*,*,#4510,.F.);
#6084=ORIENTED_EDGE('',*,*,#4511,.F.);
#6085=ORIENTED_EDGE('',*,*,#4512,.F.);
#6086=ORIENTED_EDGE('',*,*,#4513,.T.);
#6087=ORIENTED_EDGE('',*,*,#4514,.F.);
#6088=ORIENTED_EDGE('',*,*,#4515,.F.);
#6089=ORIENTED_EDGE('',*,*,#4516,.F.);
#6090=ORIENTED_EDGE('',*,*,#4504,.F.);
#6091=ORIENTED_EDGE('',*,*,#4517,.F.);
#6092=ORIENTED_EDGE('',*,*,#4518,.F.);
#6093=ORIENTED_EDGE('',*,*,#4519,.F.);
#6094=ORIENTED_EDGE('',*,*,#4468,.F.);
#6095=ORIENTED_EDGE('',*,*,#4520,.F.);
#6096=ORIENTED_EDGE('',*,*,#4521,.F.);
#6097=ORIENTED_EDGE('',*,*,#4522,.F.);
#6098=ORIENTED_EDGE('',*,*,#4486,.F.);
#6099=ORIENTED_EDGE('',*,*,#4523,.F.);
#6100=ORIENTED_EDGE('',*,*,#4495,.F.);
#6101=ORIENTED_EDGE('',*,*,#4524,.F.);
#6102=ORIENTED_EDGE('',*,*,#4525,.F.);
#6103=ORIENTED_EDGE('',*,*,#4526,.F.);
#6104=ORIENTED_EDGE('',*,*,#4477,.F.);
#6105=ORIENTED_EDGE('',*,*,#4527,.F.);
#6106=ORIENTED_EDGE('',*,*,#4528,.F.);
#6107=ORIENTED_EDGE('',*,*,#4529,.F.);
#6108=ORIENTED_EDGE('',*,*,#4513,.F.);
#6109=ORIENTED_EDGE('',*,*,#4530,.F.);
#6110=ORIENTED_EDGE('',*,*,#4531,.F.);
#6111=ORIENTED_EDGE('',*,*,#4532,.F.);
#6112=ORIENTED_EDGE('',*,*,#4531,.T.);
#6113=ORIENTED_EDGE('',*,*,#4533,.F.);
#6114=ORIENTED_EDGE('',*,*,#4534,.F.);
#6115=ORIENTED_EDGE('',*,*,#4535,.F.);
#6116=ORIENTED_EDGE('',*,*,#4536,.F.);
#6117=ORIENTED_EDGE('',*,*,#4537,.F.);
#6118=ORIENTED_EDGE('',*,*,#4538,.F.);
#6119=ORIENTED_EDGE('',*,*,#4539,.F.);
#6120=ORIENTED_EDGE('',*,*,#4540,.F.);
#6121=ORIENTED_EDGE('',*,*,#4515,.T.);
#6122=ORIENTED_EDGE('',*,*,#4541,.F.);
#6123=ORIENTED_EDGE('',*,*,#4542,.F.);
#6124=ORIENTED_EDGE('',*,*,#4543,.F.);
#6125=ORIENTED_EDGE('',*,*,#4544,.F.);
#6126=ORIENTED_EDGE('',*,*,#4545,.F.);
#6127=ORIENTED_EDGE('',*,*,#4546,.F.);
#6128=ORIENTED_EDGE('',*,*,#4547,.F.);
#6129=ORIENTED_EDGE('',*,*,#4548,.F.);
#6130=ORIENTED_EDGE('',*,*,#4525,.T.);
#6131=ORIENTED_EDGE('',*,*,#4549,.F.);
#6132=ORIENTED_EDGE('',*,*,#4550,.F.);
#6133=ORIENTED_EDGE('',*,*,#4551,.F.);
#6134=ORIENTED_EDGE('',*,*,#4552,.F.);
#6135=ORIENTED_EDGE('',*,*,#4553,.F.);
#6136=ORIENTED_EDGE('',*,*,#4554,.F.);
#6137=ORIENTED_EDGE('',*,*,#4555,.F.);
#6138=ORIENTED_EDGE('',*,*,#4556,.F.);
#6139=ORIENTED_EDGE('',*,*,#4521,.T.);
#6140=ORIENTED_EDGE('',*,*,#4557,.F.);
#6141=ORIENTED_EDGE('',*,*,#4558,.F.);
#6142=ORIENTED_EDGE('',*,*,#4559,.F.);
#6143=ORIENTED_EDGE('',*,*,#4560,.F.);
#6144=ORIENTED_EDGE('',*,*,#4561,.F.);
#6145=ORIENTED_EDGE('',*,*,#4562,.F.);
#6146=ORIENTED_EDGE('',*,*,#4563,.F.);
#6147=ORIENTED_EDGE('',*,*,#4564,.F.);
#6148=ORIENTED_EDGE('',*,*,#4528,.T.);
#6149=ORIENTED_EDGE('',*,*,#4565,.F.);
#6150=ORIENTED_EDGE('',*,*,#4566,.F.);
#6151=ORIENTED_EDGE('',*,*,#4567,.F.);
#6152=ORIENTED_EDGE('',*,*,#4568,.F.);
#6153=ORIENTED_EDGE('',*,*,#4569,.F.);
#6154=ORIENTED_EDGE('',*,*,#4570,.F.);
#6155=ORIENTED_EDGE('',*,*,#4571,.F.);
#6156=ORIENTED_EDGE('',*,*,#4572,.F.);
#6157=ORIENTED_EDGE('',*,*,#4518,.T.);
#6158=ORIENTED_EDGE('',*,*,#4573,.F.);
#6159=ORIENTED_EDGE('',*,*,#4574,.F.);
#6160=ORIENTED_EDGE('',*,*,#4575,.F.);
#6161=ORIENTED_EDGE('',*,*,#4576,.F.);
#6162=ORIENTED_EDGE('',*,*,#4577,.F.);
#6163=ORIENTED_EDGE('',*,*,#4578,.F.);
#6164=ORIENTED_EDGE('',*,*,#4579,.F.);
#6165=ORIENTED_EDGE('',*,*,#4505,.T.);
#6166=ORIENTED_EDGE('',*,*,#4516,.T.);
#6167=ORIENTED_EDGE('',*,*,#4540,.T.);
#6168=ORIENTED_EDGE('',*,*,#4580,.T.);
#6169=ORIENTED_EDGE('',*,*,#4581,.F.);
#6170=ORIENTED_EDGE('',*,*,#4582,.F.);
#6171=ORIENTED_EDGE('',*,*,#4583,.F.);
#6172=ORIENTED_EDGE('',*,*,#4584,.T.);
#6173=ORIENTED_EDGE('',*,*,#4539,.T.);
#6174=ORIENTED_EDGE('',*,*,#4585,.T.);
#6175=ORIENTED_EDGE('',*,*,#4586,.F.);
#6176=ORIENTED_EDGE('',*,*,#4580,.F.);
#6177=ORIENTED_EDGE('',*,*,#4506,.T.);
#6178=ORIENTED_EDGE('',*,*,#4584,.F.);
#6179=ORIENTED_EDGE('',*,*,#4587,.F.);
#6180=ORIENTED_EDGE('',*,*,#4588,.T.);
#6181=ORIENTED_EDGE('',*,*,#4538,.T.);
#6182=ORIENTED_EDGE('',*,*,#4589,.T.);
#6183=ORIENTED_EDGE('',*,*,#4590,.F.);
#6184=ORIENTED_EDGE('',*,*,#4585,.F.);
#6185=ORIENTED_EDGE('',*,*,#4537,.T.);
#6186=ORIENTED_EDGE('',*,*,#4591,.T.);
#6187=ORIENTED_EDGE('',*,*,#4592,.F.);
#6188=ORIENTED_EDGE('',*,*,#4589,.F.);
#6189=ORIENTED_EDGE('',*,*,#4536,.T.);
#6190=ORIENTED_EDGE('',*,*,#4593,.T.);
#6191=ORIENTED_EDGE('',*,*,#4594,.F.);
#6192=ORIENTED_EDGE('',*,*,#4591,.F.);
#6193=ORIENTED_EDGE('',*,*,#4535,.T.);
#6194=ORIENTED_EDGE('',*,*,#4595,.T.);
#6195=ORIENTED_EDGE('',*,*,#4596,.F.);
#6196=ORIENTED_EDGE('',*,*,#4593,.F.);
#6197=ORIENTED_EDGE('',*,*,#4534,.T.);
#6198=ORIENTED_EDGE('',*,*,#4597,.F.);
#6199=ORIENTED_EDGE('',*,*,#4598,.F.);
#6200=ORIENTED_EDGE('',*,*,#4595,.F.);
#6201=ORIENTED_EDGE('',*,*,#4599,.T.);
#6202=ORIENTED_EDGE('',*,*,#4600,.T.);
#6203=ORIENTED_EDGE('',*,*,#4601,.T.);
#6204=ORIENTED_EDGE('',*,*,#4602,.T.);
#6205=ORIENTED_EDGE('',*,*,#4603,.T.);
#6206=ORIENTED_EDGE('',*,*,#4604,.T.);
#6207=ORIENTED_EDGE('',*,*,#4587,.T.);
#6208=ORIENTED_EDGE('',*,*,#4583,.T.);
#6209=ORIENTED_EDGE('',*,*,#4605,.T.);
#6210=ORIENTED_EDGE('',*,*,#4606,.T.);
#6211=ORIENTED_EDGE('',*,*,#4607,.T.);
#6212=ORIENTED_EDGE('',*,*,#4608,.T.);
#6213=ORIENTED_EDGE('',*,*,#4609,.T.);
#6214=ORIENTED_EDGE('',*,*,#4610,.T.);
#6215=ORIENTED_EDGE('',*,*,#4511,.T.);
#6216=ORIENTED_EDGE('',*,*,#4611,.F.);
#6217=ORIENTED_EDGE('',*,*,#4600,.F.);
#6218=ORIENTED_EDGE('',*,*,#4612,.F.);
#6219=ORIENTED_EDGE('',*,*,#4510,.T.);
#6220=ORIENTED_EDGE('',*,*,#4613,.F.);
#6221=ORIENTED_EDGE('',*,*,#4601,.F.);
#6222=ORIENTED_EDGE('',*,*,#4611,.T.);
#6223=ORIENTED_EDGE('',*,*,#4509,.T.);
#6224=ORIENTED_EDGE('',*,*,#4614,.F.);
#6225=ORIENTED_EDGE('',*,*,#4602,.F.);
#6226=ORIENTED_EDGE('',*,*,#4613,.T.);
#6227=ORIENTED_EDGE('',*,*,#4508,.T.);
#6228=ORIENTED_EDGE('',*,*,#4615,.F.);
#6229=ORIENTED_EDGE('',*,*,#4603,.F.);
#6230=ORIENTED_EDGE('',*,*,#4614,.T.);
#6231=ORIENTED_EDGE('',*,*,#4507,.T.);
#6232=ORIENTED_EDGE('',*,*,#4588,.F.);
#6233=ORIENTED_EDGE('',*,*,#4604,.F.);
#6234=ORIENTED_EDGE('',*,*,#4615,.T.);
#6235=ORIENTED_EDGE('',*,*,#4582,.T.);
#6236=ORIENTED_EDGE('',*,*,#4616,.F.);
#6237=ORIENTED_EDGE('',*,*,#4617,.F.);
#6238=ORIENTED_EDGE('',*,*,#4605,.F.);
#6239=ORIENTED_EDGE('',*,*,#4617,.T.);
#6240=ORIENTED_EDGE('',*,*,#4618,.F.);
#6241=ORIENTED_EDGE('',*,*,#4619,.F.);
#6242=ORIENTED_EDGE('',*,*,#4606,.F.);
#6243=ORIENTED_EDGE('',*,*,#4619,.T.);
#6244=ORIENTED_EDGE('',*,*,#4620,.F.);
#6245=ORIENTED_EDGE('',*,*,#4621,.F.);
#6246=ORIENTED_EDGE('',*,*,#4607,.F.);
#6247=ORIENTED_EDGE('',*,*,#4621,.T.);
#6248=ORIENTED_EDGE('',*,*,#4622,.F.);
#6249=ORIENTED_EDGE('',*,*,#4623,.F.);
#6250=ORIENTED_EDGE('',*,*,#4608,.F.);
#6251=ORIENTED_EDGE('',*,*,#4623,.T.);
#6252=ORIENTED_EDGE('',*,*,#4624,.F.);
#6253=ORIENTED_EDGE('',*,*,#4625,.F.);
#6254=ORIENTED_EDGE('',*,*,#4609,.F.);
#6255=ORIENTED_EDGE('',*,*,#4625,.T.);
#6256=ORIENTED_EDGE('',*,*,#4626,.F.);
#6257=ORIENTED_EDGE('',*,*,#4627,.F.);
#6258=ORIENTED_EDGE('',*,*,#4610,.F.);
#6259=ORIENTED_EDGE('',*,*,#4512,.T.);
#6260=ORIENTED_EDGE('',*,*,#4612,.T.);
#6261=ORIENTED_EDGE('',*,*,#4599,.F.);
#6262=ORIENTED_EDGE('',*,*,#4627,.T.);
#6263=ORIENTED_EDGE('',*,*,#4628,.F.);
#6264=ORIENTED_EDGE('',*,*,#4597,.T.);
#6265=ORIENTED_EDGE('',*,*,#4533,.T.);
#6266=ORIENTED_EDGE('',*,*,#4530,.T.);
#6267=ORIENTED_EDGE('',*,*,#4628,.T.);
#6268=ORIENTED_EDGE('',*,*,#4626,.T.);
#6269=ORIENTED_EDGE('',*,*,#4624,.T.);
#6270=ORIENTED_EDGE('',*,*,#4622,.T.);
#6271=ORIENTED_EDGE('',*,*,#4620,.T.);
#6272=ORIENTED_EDGE('',*,*,#4618,.T.);
#6273=ORIENTED_EDGE('',*,*,#4616,.T.);
#6274=ORIENTED_EDGE('',*,*,#4581,.T.);
#6275=ORIENTED_EDGE('',*,*,#4586,.T.);
#6276=ORIENTED_EDGE('',*,*,#4590,.T.);
#6277=ORIENTED_EDGE('',*,*,#4592,.T.);
#6278=ORIENTED_EDGE('',*,*,#4594,.T.);
#6279=ORIENTED_EDGE('',*,*,#4596,.T.);
#6280=ORIENTED_EDGE('',*,*,#4598,.T.);
#6281=ORIENTED_EDGE('',*,*,#4469,.T.);
#6282=ORIENTED_EDGE('',*,*,#4519,.T.);
#6283=ORIENTED_EDGE('',*,*,#4572,.T.);
#6284=ORIENTED_EDGE('',*,*,#4629,.T.);
#6285=ORIENTED_EDGE('',*,*,#4630,.F.);
#6286=ORIENTED_EDGE('',*,*,#4631,.F.);
#6287=ORIENTED_EDGE('',*,*,#4632,.F.);
#6288=ORIENTED_EDGE('',*,*,#4633,.T.);
#6289=ORIENTED_EDGE('',*,*,#4571,.T.);
#6290=ORIENTED_EDGE('',*,*,#4634,.T.);
#6291=ORIENTED_EDGE('',*,*,#4635,.F.);
#6292=ORIENTED_EDGE('',*,*,#4629,.F.);
#6293=ORIENTED_EDGE('',*,*,#4470,.T.);
#6294=ORIENTED_EDGE('',*,*,#4633,.F.);
#6295=ORIENTED_EDGE('',*,*,#4636,.F.);
#6296=ORIENTED_EDGE('',*,*,#4637,.T.);
#6297=ORIENTED_EDGE('',*,*,#4570,.T.);
#6298=ORIENTED_EDGE('',*,*,#4638,.T.);
#6299=ORIENTED_EDGE('',*,*,#4639,.F.);
#6300=ORIENTED_EDGE('',*,*,#4634,.F.);
#6301=ORIENTED_EDGE('',*,*,#4569,.T.);
#6302=ORIENTED_EDGE('',*,*,#4640,.T.);
#6303=ORIENTED_EDGE('',*,*,#4641,.F.);
#6304=ORIENTED_EDGE('',*,*,#4638,.F.);
#6305=ORIENTED_EDGE('',*,*,#4568,.T.);
#6306=ORIENTED_EDGE('',*,*,#4642,.T.);
#6307=ORIENTED_EDGE('',*,*,#4643,.F.);
#6308=ORIENTED_EDGE('',*,*,#4640,.F.);
#6309=ORIENTED_EDGE('',*,*,#4567,.T.);
#6310=ORIENTED_EDGE('',*,*,#4644,.T.);
#6311=ORIENTED_EDGE('',*,*,#4645,.F.);
#6312=ORIENTED_EDGE('',*,*,#4642,.F.);
#6313=ORIENTED_EDGE('',*,*,#4566,.T.);
#6314=ORIENTED_EDGE('',*,*,#4646,.F.);
#6315=ORIENTED_EDGE('',*,*,#4647,.F.);
#6316=ORIENTED_EDGE('',*,*,#4644,.F.);
#6317=ORIENTED_EDGE('',*,*,#4648,.T.);
#6318=ORIENTED_EDGE('',*,*,#4649,.T.);
#6319=ORIENTED_EDGE('',*,*,#4650,.T.);
#6320=ORIENTED_EDGE('',*,*,#4651,.T.);
#6321=ORIENTED_EDGE('',*,*,#4652,.T.);
#6322=ORIENTED_EDGE('',*,*,#4653,.T.);
#6323=ORIENTED_EDGE('',*,*,#4636,.T.);
#6324=ORIENTED_EDGE('',*,*,#4632,.T.);
#6325=ORIENTED_EDGE('',*,*,#4654,.T.);
#6326=ORIENTED_EDGE('',*,*,#4655,.T.);
#6327=ORIENTED_EDGE('',*,*,#4656,.T.);
#6328=ORIENTED_EDGE('',*,*,#4657,.T.);
#6329=ORIENTED_EDGE('',*,*,#4658,.T.);
#6330=ORIENTED_EDGE('',*,*,#4659,.T.);
#6331=ORIENTED_EDGE('',*,*,#4475,.T.);
#6332=ORIENTED_EDGE('',*,*,#4660,.F.);
#6333=ORIENTED_EDGE('',*,*,#4649,.F.);
#6334=ORIENTED_EDGE('',*,*,#4661,.F.);
#6335=ORIENTED_EDGE('',*,*,#4474,.T.);
#6336=ORIENTED_EDGE('',*,*,#4662,.F.);
#6337=ORIENTED_EDGE('',*,*,#4650,.F.);
#6338=ORIENTED_EDGE('',*,*,#4660,.T.);
#6339=ORIENTED_EDGE('',*,*,#4473,.T.);
#6340=ORIENTED_EDGE('',*,*,#4663,.F.);
#6341=ORIENTED_EDGE('',*,*,#4651,.F.);
#6342=ORIENTED_EDGE('',*,*,#4662,.T.);
#6343=ORIENTED_EDGE('',*,*,#4472,.T.);
#6344=ORIENTED_EDGE('',*,*,#4664,.F.);
#6345=ORIENTED_EDGE('',*,*,#4652,.F.);
#6346=ORIENTED_EDGE('',*,*,#4663,.T.);
#6347=ORIENTED_EDGE('',*,*,#4471,.T.);
#6348=ORIENTED_EDGE('',*,*,#4637,.F.);
#6349=ORIENTED_EDGE('',*,*,#4653,.F.);
#6350=ORIENTED_EDGE('',*,*,#4664,.T.);
#6351=ORIENTED_EDGE('',*,*,#4631,.T.);
#6352=ORIENTED_EDGE('',*,*,#4665,.F.);
#6353=ORIENTED_EDGE('',*,*,#4666,.F.);
#6354=ORIENTED_EDGE('',*,*,#4654,.F.);
#6355=ORIENTED_EDGE('',*,*,#4666,.T.);
#6356=ORIENTED_EDGE('',*,*,#4667,.F.);
#6357=ORIENTED_EDGE('',*,*,#4668,.F.);
#6358=ORIENTED_EDGE('',*,*,#4655,.F.);
#6359=ORIENTED_EDGE('',*,*,#4668,.T.);
#6360=ORIENTED_EDGE('',*,*,#4669,.F.);
#6361=ORIENTED_EDGE('',*,*,#4670,.F.);
#6362=ORIENTED_EDGE('',*,*,#4656,.F.);
#6363=ORIENTED_EDGE('',*,*,#4670,.T.);
#6364=ORIENTED_EDGE('',*,*,#4671,.F.);
#6365=ORIENTED_EDGE('',*,*,#4672,.F.);
#6366=ORIENTED_EDGE('',*,*,#4657,.F.);
#6367=ORIENTED_EDGE('',*,*,#4672,.T.);
#6368=ORIENTED_EDGE('',*,*,#4673,.F.);
#6369=ORIENTED_EDGE('',*,*,#4674,.F.);
#6370=ORIENTED_EDGE('',*,*,#4658,.F.);
#6371=ORIENTED_EDGE('',*,*,#4674,.T.);
#6372=ORIENTED_EDGE('',*,*,#4675,.F.);
#6373=ORIENTED_EDGE('',*,*,#4676,.F.);
#6374=ORIENTED_EDGE('',*,*,#4659,.F.);
#6375=ORIENTED_EDGE('',*,*,#4476,.T.);
#6376=ORIENTED_EDGE('',*,*,#4661,.T.);
#6377=ORIENTED_EDGE('',*,*,#4648,.F.);
#6378=ORIENTED_EDGE('',*,*,#4676,.T.);
#6379=ORIENTED_EDGE('',*,*,#4677,.F.);
#6380=ORIENTED_EDGE('',*,*,#4646,.T.);
#6381=ORIENTED_EDGE('',*,*,#4565,.T.);
#6382=ORIENTED_EDGE('',*,*,#4527,.T.);
#6383=ORIENTED_EDGE('',*,*,#4677,.T.);
#6384=ORIENTED_EDGE('',*,*,#4675,.T.);
#6385=ORIENTED_EDGE('',*,*,#4673,.T.);
#6386=ORIENTED_EDGE('',*,*,#4671,.T.);
#6387=ORIENTED_EDGE('',*,*,#4669,.T.);
#6388=ORIENTED_EDGE('',*,*,#4667,.T.);
#6389=ORIENTED_EDGE('',*,*,#4665,.T.);
#6390=ORIENTED_EDGE('',*,*,#4630,.T.);
#6391=ORIENTED_EDGE('',*,*,#4635,.T.);
#6392=ORIENTED_EDGE('',*,*,#4639,.T.);
#6393=ORIENTED_EDGE('',*,*,#4641,.T.);
#6394=ORIENTED_EDGE('',*,*,#4643,.T.);
#6395=ORIENTED_EDGE('',*,*,#4645,.T.);
#6396=ORIENTED_EDGE('',*,*,#4647,.T.);
#6397=ORIENTED_EDGE('',*,*,#4487,.T.);
#6398=ORIENTED_EDGE('',*,*,#4522,.T.);
#6399=ORIENTED_EDGE('',*,*,#4556,.T.);
#6400=ORIENTED_EDGE('',*,*,#4678,.T.);
#6401=ORIENTED_EDGE('',*,*,#4679,.F.);
#6402=ORIENTED_EDGE('',*,*,#4680,.F.);
#6403=ORIENTED_EDGE('',*,*,#4681,.F.);
#6404=ORIENTED_EDGE('',*,*,#4682,.T.);
#6405=ORIENTED_EDGE('',*,*,#4555,.T.);
#6406=ORIENTED_EDGE('',*,*,#4683,.T.);
#6407=ORIENTED_EDGE('',*,*,#4684,.F.);
#6408=ORIENTED_EDGE('',*,*,#4678,.F.);
#6409=ORIENTED_EDGE('',*,*,#4488,.T.);
#6410=ORIENTED_EDGE('',*,*,#4682,.F.);
#6411=ORIENTED_EDGE('',*,*,#4685,.F.);
#6412=ORIENTED_EDGE('',*,*,#4686,.T.);
#6413=ORIENTED_EDGE('',*,*,#4554,.T.);
#6414=ORIENTED_EDGE('',*,*,#4687,.T.);
#6415=ORIENTED_EDGE('',*,*,#4688,.F.);
#6416=ORIENTED_EDGE('',*,*,#4683,.F.);
#6417=ORIENTED_EDGE('',*,*,#4553,.T.);
#6418=ORIENTED_EDGE('',*,*,#4689,.T.);
#6419=ORIENTED_EDGE('',*,*,#4690,.F.);
#6420=ORIENTED_EDGE('',*,*,#4687,.F.);
#6421=ORIENTED_EDGE('',*,*,#4552,.T.);
#6422=ORIENTED_EDGE('',*,*,#4691,.T.);
#6423=ORIENTED_EDGE('',*,*,#4692,.F.);
#6424=ORIENTED_EDGE('',*,*,#4689,.F.);
#6425=ORIENTED_EDGE('',*,*,#4551,.T.);
#6426=ORIENTED_EDGE('',*,*,#4693,.T.);
#6427=ORIENTED_EDGE('',*,*,#4694,.F.);
#6428=ORIENTED_EDGE('',*,*,#4691,.F.);
#6429=ORIENTED_EDGE('',*,*,#4550,.T.);
#6430=ORIENTED_EDGE('',*,*,#4695,.F.);
#6431=ORIENTED_EDGE('',*,*,#4696,.F.);
#6432=ORIENTED_EDGE('',*,*,#4693,.F.);
#6433=ORIENTED_EDGE('',*,*,#4697,.T.);
#6434=ORIENTED_EDGE('',*,*,#4698,.T.);
#6435=ORIENTED_EDGE('',*,*,#4699,.T.);
#6436=ORIENTED_EDGE('',*,*,#4700,.T.);
#6437=ORIENTED_EDGE('',*,*,#4701,.T.);
#6438=ORIENTED_EDGE('',*,*,#4702,.T.);
#6439=ORIENTED_EDGE('',*,*,#4685,.T.);
#6440=ORIENTED_EDGE('',*,*,#4681,.T.);
#6441=ORIENTED_EDGE('',*,*,#4703,.T.);
#6442=ORIENTED_EDGE('',*,*,#4704,.T.);
#6443=ORIENTED_EDGE('',*,*,#4705,.T.);
#6444=ORIENTED_EDGE('',*,*,#4706,.T.);
#6445=ORIENTED_EDGE('',*,*,#4707,.T.);
#6446=ORIENTED_EDGE('',*,*,#4708,.T.);
#6447=ORIENTED_EDGE('',*,*,#4493,.T.);
#6448=ORIENTED_EDGE('',*,*,#4709,.F.);
#6449=ORIENTED_EDGE('',*,*,#4698,.F.);
#6450=ORIENTED_EDGE('',*,*,#4710,.F.);
#6451=ORIENTED_EDGE('',*,*,#4492,.T.);
#6452=ORIENTED_EDGE('',*,*,#4711,.F.);
#6453=ORIENTED_EDGE('',*,*,#4699,.F.);
#6454=ORIENTED_EDGE('',*,*,#4709,.T.);
#6455=ORIENTED_EDGE('',*,*,#4491,.T.);
#6456=ORIENTED_EDGE('',*,*,#4712,.F.);
#6457=ORIENTED_EDGE('',*,*,#4700,.F.);
#6458=ORIENTED_EDGE('',*,*,#4711,.T.);
#6459=ORIENTED_EDGE('',*,*,#4490,.T.);
#6460=ORIENTED_EDGE('',*,*,#4713,.F.);
#6461=ORIENTED_EDGE('',*,*,#4701,.F.);
#6462=ORIENTED_EDGE('',*,*,#4712,.T.);
#6463=ORIENTED_EDGE('',*,*,#4489,.T.);
#6464=ORIENTED_EDGE('',*,*,#4686,.F.);
#6465=ORIENTED_EDGE('',*,*,#4702,.F.);
#6466=ORIENTED_EDGE('',*,*,#4713,.T.);
#6467=ORIENTED_EDGE('',*,*,#4680,.T.);
#6468=ORIENTED_EDGE('',*,*,#4714,.F.);
#6469=ORIENTED_EDGE('',*,*,#4715,.F.);
#6470=ORIENTED_EDGE('',*,*,#4703,.F.);
#6471=ORIENTED_EDGE('',*,*,#4715,.T.);
#6472=ORIENTED_EDGE('',*,*,#4716,.F.);
#6473=ORIENTED_EDGE('',*,*,#4717,.F.);
#6474=ORIENTED_EDGE('',*,*,#4704,.F.);
#6475=ORIENTED_EDGE('',*,*,#4717,.T.);
#6476=ORIENTED_EDGE('',*,*,#4718,.F.);
#6477=ORIENTED_EDGE('',*,*,#4719,.F.);
#6478=ORIENTED_EDGE('',*,*,#4705,.F.);
#6479=ORIENTED_EDGE('',*,*,#4719,.T.);
#6480=ORIENTED_EDGE('',*,*,#4720,.F.);
#6481=ORIENTED_EDGE('',*,*,#4721,.F.);
#6482=ORIENTED_EDGE('',*,*,#4706,.F.);
#6483=ORIENTED_EDGE('',*,*,#4721,.T.);
#6484=ORIENTED_EDGE('',*,*,#4722,.F.);
#6485=ORIENTED_EDGE('',*,*,#4723,.F.);
#6486=ORIENTED_EDGE('',*,*,#4707,.F.);
#6487=ORIENTED_EDGE('',*,*,#4723,.T.);
#6488=ORIENTED_EDGE('',*,*,#4724,.F.);
#6489=ORIENTED_EDGE('',*,*,#4725,.F.);
#6490=ORIENTED_EDGE('',*,*,#4708,.F.);
#6491=ORIENTED_EDGE('',*,*,#4494,.T.);
#6492=ORIENTED_EDGE('',*,*,#4710,.T.);
#6493=ORIENTED_EDGE('',*,*,#4697,.F.);
#6494=ORIENTED_EDGE('',*,*,#4725,.T.);
#6495=ORIENTED_EDGE('',*,*,#4726,.F.);
#6496=ORIENTED_EDGE('',*,*,#4695,.T.);
#6497=ORIENTED_EDGE('',*,*,#4549,.T.);
#6498=ORIENTED_EDGE('',*,*,#4524,.T.);
#6499=ORIENTED_EDGE('',*,*,#4726,.T.);
#6500=ORIENTED_EDGE('',*,*,#4724,.T.);
#6501=ORIENTED_EDGE('',*,*,#4722,.T.);
#6502=ORIENTED_EDGE('',*,*,#4720,.T.);
#6503=ORIENTED_EDGE('',*,*,#4718,.T.);
#6504=ORIENTED_EDGE('',*,*,#4716,.T.);
#6505=ORIENTED_EDGE('',*,*,#4714,.T.);
#6506=ORIENTED_EDGE('',*,*,#4679,.T.);
#6507=ORIENTED_EDGE('',*,*,#4684,.T.);
#6508=ORIENTED_EDGE('',*,*,#4688,.T.);
#6509=ORIENTED_EDGE('',*,*,#4690,.T.);
#6510=ORIENTED_EDGE('',*,*,#4692,.T.);
#6511=ORIENTED_EDGE('',*,*,#4694,.T.);
#6512=ORIENTED_EDGE('',*,*,#4696,.T.);
#6513=ORIENTED_EDGE('',*,*,#4496,.T.);
#6514=ORIENTED_EDGE('',*,*,#4523,.T.);
#6515=ORIENTED_EDGE('',*,*,#4548,.T.);
#6516=ORIENTED_EDGE('',*,*,#4727,.T.);
#6517=ORIENTED_EDGE('',*,*,#4728,.F.);
#6518=ORIENTED_EDGE('',*,*,#4729,.F.);
#6519=ORIENTED_EDGE('',*,*,#4730,.F.);
#6520=ORIENTED_EDGE('',*,*,#4731,.T.);
#6521=ORIENTED_EDGE('',*,*,#4547,.T.);
#6522=ORIENTED_EDGE('',*,*,#4732,.T.);
#6523=ORIENTED_EDGE('',*,*,#4733,.F.);
#6524=ORIENTED_EDGE('',*,*,#4727,.F.);
#6525=ORIENTED_EDGE('',*,*,#4497,.T.);
#6526=ORIENTED_EDGE('',*,*,#4731,.F.);
#6527=ORIENTED_EDGE('',*,*,#4734,.F.);
#6528=ORIENTED_EDGE('',*,*,#4735,.T.);
#6529=ORIENTED_EDGE('',*,*,#4546,.T.);
#6530=ORIENTED_EDGE('',*,*,#4736,.T.);
#6531=ORIENTED_EDGE('',*,*,#4737,.F.);
#6532=ORIENTED_EDGE('',*,*,#4732,.F.);
#6533=ORIENTED_EDGE('',*,*,#4545,.T.);
#6534=ORIENTED_EDGE('',*,*,#4738,.T.);
#6535=ORIENTED_EDGE('',*,*,#4739,.F.);
#6536=ORIENTED_EDGE('',*,*,#4736,.F.);
#6537=ORIENTED_EDGE('',*,*,#4544,.T.);
#6538=ORIENTED_EDGE('',*,*,#4740,.T.);
#6539=ORIENTED_EDGE('',*,*,#4741,.F.);
#6540=ORIENTED_EDGE('',*,*,#4738,.F.);
#6541=ORIENTED_EDGE('',*,*,#4543,.T.);
#6542=ORIENTED_EDGE('',*,*,#4742,.T.);
#6543=ORIENTED_EDGE('',*,*,#4743,.F.);
#6544=ORIENTED_EDGE('',*,*,#4740,.F.);
#6545=ORIENTED_EDGE('',*,*,#4542,.T.);
#6546=ORIENTED_EDGE('',*,*,#4744,.F.);
#6547=ORIENTED_EDGE('',*,*,#4745,.F.);
#6548=ORIENTED_EDGE('',*,*,#4742,.F.);
#6549=ORIENTED_EDGE('',*,*,#4746,.T.);
#6550=ORIENTED_EDGE('',*,*,#4747,.T.);
#6551=ORIENTED_EDGE('',*,*,#4748,.T.);
#6552=ORIENTED_EDGE('',*,*,#4749,.T.);
#6553=ORIENTED_EDGE('',*,*,#4750,.T.);
#6554=ORIENTED_EDGE('',*,*,#4751,.T.);
#6555=ORIENTED_EDGE('',*,*,#4734,.T.);
#6556=ORIENTED_EDGE('',*,*,#4730,.T.);
#6557=ORIENTED_EDGE('',*,*,#4752,.T.);
#6558=ORIENTED_EDGE('',*,*,#4753,.T.);
#6559=ORIENTED_EDGE('',*,*,#4754,.T.);
#6560=ORIENTED_EDGE('',*,*,#4755,.T.);
#6561=ORIENTED_EDGE('',*,*,#4756,.T.);
#6562=ORIENTED_EDGE('',*,*,#4757,.T.);
#6563=ORIENTED_EDGE('',*,*,#4502,.T.);
#6564=ORIENTED_EDGE('',*,*,#4758,.F.);
#6565=ORIENTED_EDGE('',*,*,#4747,.F.);
#6566=ORIENTED_EDGE('',*,*,#4759,.F.);
#6567=ORIENTED_EDGE('',*,*,#4501,.T.);
#6568=ORIENTED_EDGE('',*,*,#4760,.F.);
#6569=ORIENTED_EDGE('',*,*,#4748,.F.);
#6570=ORIENTED_EDGE('',*,*,#4758,.T.);
#6571=ORIENTED_EDGE('',*,*,#4500,.T.);
#6572=ORIENTED_EDGE('',*,*,#4761,.F.);
#6573=ORIENTED_EDGE('',*,*,#4749,.F.);
#6574=ORIENTED_EDGE('',*,*,#4760,.T.);
#6575=ORIENTED_EDGE('',*,*,#4499,.T.);
#6576=ORIENTED_EDGE('',*,*,#4762,.F.);
#6577=ORIENTED_EDGE('',*,*,#4750,.F.);
#6578=ORIENTED_EDGE('',*,*,#4761,.T.);
#6579=ORIENTED_EDGE('',*,*,#4498,.T.);
#6580=ORIENTED_EDGE('',*,*,#4735,.F.);
#6581=ORIENTED_EDGE('',*,*,#4751,.F.);
#6582=ORIENTED_EDGE('',*,*,#4762,.T.);
#6583=ORIENTED_EDGE('',*,*,#4729,.T.);
#6584=ORIENTED_EDGE('',*,*,#4763,.F.);
#6585=ORIENTED_EDGE('',*,*,#4764,.F.);
#6586=ORIENTED_EDGE('',*,*,#4752,.F.);
#6587=ORIENTED_EDGE('',*,*,#4764,.T.);
#6588=ORIENTED_EDGE('',*,*,#4765,.F.);
#6589=ORIENTED_EDGE('',*,*,#4766,.F.);
#6590=ORIENTED_EDGE('',*,*,#4753,.F.);
#6591=ORIENTED_EDGE('',*,*,#4766,.T.);
#6592=ORIENTED_EDGE('',*,*,#4767,.F.);
#6593=ORIENTED_EDGE('',*,*,#4768,.F.);
#6594=ORIENTED_EDGE('',*,*,#4754,.F.);
#6595=ORIENTED_EDGE('',*,*,#4768,.T.);
#6596=ORIENTED_EDGE('',*,*,#4769,.F.);
#6597=ORIENTED_EDGE('',*,*,#4770,.F.);
#6598=ORIENTED_EDGE('',*,*,#4755,.F.);
#6599=ORIENTED_EDGE('',*,*,#4770,.T.);
#6600=ORIENTED_EDGE('',*,*,#4771,.F.);
#6601=ORIENTED_EDGE('',*,*,#4772,.F.);
#6602=ORIENTED_EDGE('',*,*,#4756,.F.);
#6603=ORIENTED_EDGE('',*,*,#4772,.T.);
#6604=ORIENTED_EDGE('',*,*,#4773,.F.);
#6605=ORIENTED_EDGE('',*,*,#4774,.F.);
#6606=ORIENTED_EDGE('',*,*,#4757,.F.);
#6607=ORIENTED_EDGE('',*,*,#4503,.T.);
#6608=ORIENTED_EDGE('',*,*,#4759,.T.);
#6609=ORIENTED_EDGE('',*,*,#4746,.F.);
#6610=ORIENTED_EDGE('',*,*,#4774,.T.);
#6611=ORIENTED_EDGE('',*,*,#4775,.F.);
#6612=ORIENTED_EDGE('',*,*,#4744,.T.);
#6613=ORIENTED_EDGE('',*,*,#4541,.T.);
#6614=ORIENTED_EDGE('',*,*,#4514,.T.);
#6615=ORIENTED_EDGE('',*,*,#4775,.T.);
#6616=ORIENTED_EDGE('',*,*,#4773,.T.);
#6617=ORIENTED_EDGE('',*,*,#4771,.T.);
#6618=ORIENTED_EDGE('',*,*,#4769,.T.);
#6619=ORIENTED_EDGE('',*,*,#4767,.T.);
#6620=ORIENTED_EDGE('',*,*,#4765,.T.);
#6621=ORIENTED_EDGE('',*,*,#4763,.T.);
#6622=ORIENTED_EDGE('',*,*,#4728,.T.);
#6623=ORIENTED_EDGE('',*,*,#4733,.T.);
#6624=ORIENTED_EDGE('',*,*,#4737,.T.);
#6625=ORIENTED_EDGE('',*,*,#4739,.T.);
#6626=ORIENTED_EDGE('',*,*,#4741,.T.);
#6627=ORIENTED_EDGE('',*,*,#4743,.T.);
#6628=ORIENTED_EDGE('',*,*,#4745,.T.);
#6629=ORIENTED_EDGE('',*,*,#4478,.T.);
#6630=ORIENTED_EDGE('',*,*,#4526,.T.);
#6631=ORIENTED_EDGE('',*,*,#4564,.T.);
#6632=ORIENTED_EDGE('',*,*,#4776,.T.);
#6633=ORIENTED_EDGE('',*,*,#4777,.F.);
#6634=ORIENTED_EDGE('',*,*,#4778,.F.);
#6635=ORIENTED_EDGE('',*,*,#4779,.F.);
#6636=ORIENTED_EDGE('',*,*,#4780,.T.);
#6637=ORIENTED_EDGE('',*,*,#4563,.T.);
#6638=ORIENTED_EDGE('',*,*,#4781,.T.);
#6639=ORIENTED_EDGE('',*,*,#4782,.F.);
#6640=ORIENTED_EDGE('',*,*,#4776,.F.);
#6641=ORIENTED_EDGE('',*,*,#4479,.T.);
#6642=ORIENTED_EDGE('',*,*,#4780,.F.);
#6643=ORIENTED_EDGE('',*,*,#4783,.F.);
#6644=ORIENTED_EDGE('',*,*,#4784,.T.);
#6645=ORIENTED_EDGE('',*,*,#4562,.T.);
#6646=ORIENTED_EDGE('',*,*,#4785,.T.);
#6647=ORIENTED_EDGE('',*,*,#4786,.F.);
#6648=ORIENTED_EDGE('',*,*,#4781,.F.);
#6649=ORIENTED_EDGE('',*,*,#4561,.T.);
#6650=ORIENTED_EDGE('',*,*,#4787,.T.);
#6651=ORIENTED_EDGE('',*,*,#4788,.F.);
#6652=ORIENTED_EDGE('',*,*,#4785,.F.);
#6653=ORIENTED_EDGE('',*,*,#4560,.T.);
#6654=ORIENTED_EDGE('',*,*,#4789,.T.);
#6655=ORIENTED_EDGE('',*,*,#4790,.F.);
#6656=ORIENTED_EDGE('',*,*,#4787,.F.);
#6657=ORIENTED_EDGE('',*,*,#4559,.T.);
#6658=ORIENTED_EDGE('',*,*,#4791,.T.);
#6659=ORIENTED_EDGE('',*,*,#4792,.F.);
#6660=ORIENTED_EDGE('',*,*,#4789,.F.);
#6661=ORIENTED_EDGE('',*,*,#4558,.T.);
#6662=ORIENTED_EDGE('',*,*,#4793,.F.);
#6663=ORIENTED_EDGE('',*,*,#4794,.F.);
#6664=ORIENTED_EDGE('',*,*,#4791,.F.);
#6665=ORIENTED_EDGE('',*,*,#4795,.T.);
#6666=ORIENTED_EDGE('',*,*,#4796,.T.);
#6667=ORIENTED_EDGE('',*,*,#4797,.T.);
#6668=ORIENTED_EDGE('',*,*,#4798,.T.);
#6669=ORIENTED_EDGE('',*,*,#4799,.T.);
#6670=ORIENTED_EDGE('',*,*,#4800,.T.);
#6671=ORIENTED_EDGE('',*,*,#4783,.T.);
#6672=ORIENTED_EDGE('',*,*,#4779,.T.);
#6673=ORIENTED_EDGE('',*,*,#4801,.T.);
#6674=ORIENTED_EDGE('',*,*,#4802,.T.);
#6675=ORIENTED_EDGE('',*,*,#4803,.T.);
#6676=ORIENTED_EDGE('',*,*,#4804,.T.);
#6677=ORIENTED_EDGE('',*,*,#4805,.T.);
#6678=ORIENTED_EDGE('',*,*,#4806,.T.);
#6679=ORIENTED_EDGE('',*,*,#4484,.T.);
#6680=ORIENTED_EDGE('',*,*,#4807,.F.);
#6681=ORIENTED_EDGE('',*,*,#4796,.F.);
#6682=ORIENTED_EDGE('',*,*,#4808,.F.);
#6683=ORIENTED_EDGE('',*,*,#4483,.T.);
#6684=ORIENTED_EDGE('',*,*,#4809,.F.);
#6685=ORIENTED_EDGE('',*,*,#4797,.F.);
#6686=ORIENTED_EDGE('',*,*,#4807,.T.);
#6687=ORIENTED_EDGE('',*,*,#4482,.T.);
#6688=ORIENTED_EDGE('',*,*,#4810,.F.);
#6689=ORIENTED_EDGE('',*,*,#4798,.F.);
#6690=ORIENTED_EDGE('',*,*,#4809,.T.);
#6691=ORIENTED_EDGE('',*,*,#4481,.T.);
#6692=ORIENTED_EDGE('',*,*,#4811,.F.);
#6693=ORIENTED_EDGE('',*,*,#4799,.F.);
#6694=ORIENTED_EDGE('',*,*,#4810,.T.);
#6695=ORIENTED_EDGE('',*,*,#4480,.T.);
#6696=ORIENTED_EDGE('',*,*,#4784,.F.);
#6697=ORIENTED_EDGE('',*,*,#4800,.F.);
#6698=ORIENTED_EDGE('',*,*,#4811,.T.);
#6699=ORIENTED_EDGE('',*,*,#4778,.T.);
#6700=ORIENTED_EDGE('',*,*,#4812,.F.);
#6701=ORIENTED_EDGE('',*,*,#4813,.F.);
#6702=ORIENTED_EDGE('',*,*,#4801,.F.);
#6703=ORIENTED_EDGE('',*,*,#4813,.T.);
#6704=ORIENTED_EDGE('',*,*,#4814,.F.);
#6705=ORIENTED_EDGE('',*,*,#4815,.F.);
#6706=ORIENTED_EDGE('',*,*,#4802,.F.);
#6707=ORIENTED_EDGE('',*,*,#4815,.T.);
#6708=ORIENTED_EDGE('',*,*,#4816,.F.);
#6709=ORIENTED_EDGE('',*,*,#4817,.F.);
#6710=ORIENTED_EDGE('',*,*,#4803,.F.);
#6711=ORIENTED_EDGE('',*,*,#4817,.T.);
#6712=ORIENTED_EDGE('',*,*,#4818,.F.);
#6713=ORIENTED_EDGE('',*,*,#4819,.F.);
#6714=ORIENTED_EDGE('',*,*,#4804,.F.);
#6715=ORIENTED_EDGE('',*,*,#4819,.T.);
#6716=ORIENTED_EDGE('',*,*,#4820,.F.);
#6717=ORIENTED_EDGE('',*,*,#4821,.F.);
#6718=ORIENTED_EDGE('',*,*,#4805,.F.);
#6719=ORIENTED_EDGE('',*,*,#4821,.T.);
#6720=ORIENTED_EDGE('',*,*,#4822,.F.);
#6721=ORIENTED_EDGE('',*,*,#4823,.F.);
#6722=ORIENTED_EDGE('',*,*,#4806,.F.);
#6723=ORIENTED_EDGE('',*,*,#4485,.T.);
#6724=ORIENTED_EDGE('',*,*,#4808,.T.);
#6725=ORIENTED_EDGE('',*,*,#4795,.F.);
#6726=ORIENTED_EDGE('',*,*,#4823,.T.);
#6727=ORIENTED_EDGE('',*,*,#4824,.F.);
#6728=ORIENTED_EDGE('',*,*,#4793,.T.);
#6729=ORIENTED_EDGE('',*,*,#4557,.T.);
#6730=ORIENTED_EDGE('',*,*,#4520,.T.);
#6731=ORIENTED_EDGE('',*,*,#4824,.T.);
#6732=ORIENTED_EDGE('',*,*,#4822,.T.);
#6733=ORIENTED_EDGE('',*,*,#4820,.T.);
#6734=ORIENTED_EDGE('',*,*,#4818,.T.);
#6735=ORIENTED_EDGE('',*,*,#4816,.T.);
#6736=ORIENTED_EDGE('',*,*,#4814,.T.);
#6737=ORIENTED_EDGE('',*,*,#4812,.T.);
#6738=ORIENTED_EDGE('',*,*,#4777,.T.);
#6739=ORIENTED_EDGE('',*,*,#4782,.T.);
#6740=ORIENTED_EDGE('',*,*,#4786,.T.);
#6741=ORIENTED_EDGE('',*,*,#4788,.T.);
#6742=ORIENTED_EDGE('',*,*,#4790,.T.);
#6743=ORIENTED_EDGE('',*,*,#4792,.T.);
#6744=ORIENTED_EDGE('',*,*,#4794,.T.);
#6745=ORIENTED_EDGE('',*,*,#4460,.T.);
#6746=ORIENTED_EDGE('',*,*,#4529,.T.);
#6747=ORIENTED_EDGE('',*,*,#4532,.T.);
#6748=ORIENTED_EDGE('',*,*,#4825,.T.);
#6749=ORIENTED_EDGE('',*,*,#4826,.F.);
#6750=ORIENTED_EDGE('',*,*,#4827,.F.);
#6751=ORIENTED_EDGE('',*,*,#4828,.F.);
#6752=ORIENTED_EDGE('',*,*,#4829,.T.);
#6753=ORIENTED_EDGE('',*,*,#4579,.T.);
#6754=ORIENTED_EDGE('',*,*,#4830,.T.);
#6755=ORIENTED_EDGE('',*,*,#4831,.F.);
#6756=ORIENTED_EDGE('',*,*,#4825,.F.);
#6757=ORIENTED_EDGE('',*,*,#4461,.T.);
#6758=ORIENTED_EDGE('',*,*,#4829,.F.);
#6759=ORIENTED_EDGE('',*,*,#4832,.F.);
#6760=ORIENTED_EDGE('',*,*,#4833,.T.);
#6761=ORIENTED_EDGE('',*,*,#4578,.T.);
#6762=ORIENTED_EDGE('',*,*,#4834,.T.);
#6763=ORIENTED_EDGE('',*,*,#4835,.F.);
#6764=ORIENTED_EDGE('',*,*,#4830,.F.);
#6765=ORIENTED_EDGE('',*,*,#4577,.T.);
#6766=ORIENTED_EDGE('',*,*,#4836,.T.);
#6767=ORIENTED_EDGE('',*,*,#4837,.F.);
#6768=ORIENTED_EDGE('',*,*,#4834,.F.);
#6769=ORIENTED_EDGE('',*,*,#4576,.T.);
#6770=ORIENTED_EDGE('',*,*,#4838,.T.);
#6771=ORIENTED_EDGE('',*,*,#4839,.F.);
#6772=ORIENTED_EDGE('',*,*,#4836,.F.);
#6773=ORIENTED_EDGE('',*,*,#4575,.T.);
#6774=ORIENTED_EDGE('',*,*,#4840,.T.);
#6775=ORIENTED_EDGE('',*,*,#4841,.F.);
#6776=ORIENTED_EDGE('',*,*,#4838,.F.);
#6777=ORIENTED_EDGE('',*,*,#4574,.T.);
#6778=ORIENTED_EDGE('',*,*,#4842,.F.);
#6779=ORIENTED_EDGE('',*,*,#4843,.F.);
#6780=ORIENTED_EDGE('',*,*,#4840,.F.);
#6781=ORIENTED_EDGE('',*,*,#4844,.T.);
#6782=ORIENTED_EDGE('',*,*,#4845,.T.);
#6783=ORIENTED_EDGE('',*,*,#4846,.T.);
#6784=ORIENTED_EDGE('',*,*,#4847,.T.);
#6785=ORIENTED_EDGE('',*,*,#4848,.T.);
#6786=ORIENTED_EDGE('',*,*,#4849,.T.);
#6787=ORIENTED_EDGE('',*,*,#4832,.T.);
#6788=ORIENTED_EDGE('',*,*,#4828,.T.);
#6789=ORIENTED_EDGE('',*,*,#4850,.T.);
#6790=ORIENTED_EDGE('',*,*,#4851,.T.);
#6791=ORIENTED_EDGE('',*,*,#4852,.T.);
#6792=ORIENTED_EDGE('',*,*,#4853,.T.);
#6793=ORIENTED_EDGE('',*,*,#4854,.T.);
#6794=ORIENTED_EDGE('',*,*,#4855,.T.);
#6795=ORIENTED_EDGE('',*,*,#4466,.T.);
#6796=ORIENTED_EDGE('',*,*,#4856,.F.);
#6797=ORIENTED_EDGE('',*,*,#4845,.F.);
#6798=ORIENTED_EDGE('',*,*,#4857,.F.);
#6799=ORIENTED_EDGE('',*,*,#4465,.T.);
#6800=ORIENTED_EDGE('',*,*,#4858,.F.);
#6801=ORIENTED_EDGE('',*,*,#4846,.F.);
#6802=ORIENTED_EDGE('',*,*,#4856,.T.);
#6803=ORIENTED_EDGE('',*,*,#4464,.T.);
#6804=ORIENTED_EDGE('',*,*,#4859,.F.);
#6805=ORIENTED_EDGE('',*,*,#4847,.F.);
#6806=ORIENTED_EDGE('',*,*,#4858,.T.);
#6807=ORIENTED_EDGE('',*,*,#4463,.T.);
#6808=ORIENTED_EDGE('',*,*,#4860,.F.);
#6809=ORIENTED_EDGE('',*,*,#4848,.F.);
#6810=ORIENTED_EDGE('',*,*,#4859,.T.);
#6811=ORIENTED_EDGE('',*,*,#4462,.T.);
#6812=ORIENTED_EDGE('',*,*,#4833,.F.);
#6813=ORIENTED_EDGE('',*,*,#4849,.F.);
#6814=ORIENTED_EDGE('',*,*,#4860,.T.);
#6815=ORIENTED_EDGE('',*,*,#4827,.T.);
#6816=ORIENTED_EDGE('',*,*,#4861,.F.);
#6817=ORIENTED_EDGE('',*,*,#4862,.F.);
#6818=ORIENTED_EDGE('',*,*,#4850,.F.);
#6819=ORIENTED_EDGE('',*,*,#4862,.T.);
#6820=ORIENTED_EDGE('',*,*,#4863,.F.);
#6821=ORIENTED_EDGE('',*,*,#4864,.F.);
#6822=ORIENTED_EDGE('',*,*,#4851,.F.);
#6823=ORIENTED_EDGE('',*,*,#4864,.T.);
#6824=ORIENTED_EDGE('',*,*,#4865,.F.);
#6825=ORIENTED_EDGE('',*,*,#4866,.F.);
#6826=ORIENTED_EDGE('',*,*,#4852,.F.);
#6827=ORIENTED_EDGE('',*,*,#4866,.T.);
#6828=ORIENTED_EDGE('',*,*,#4867,.F.);
#6829=ORIENTED_EDGE('',*,*,#4868,.F.);
#6830=ORIENTED_EDGE('',*,*,#4853,.F.);
#6831=ORIENTED_EDGE('',*,*,#4868,.T.);
#6832=ORIENTED_EDGE('',*,*,#4869,.F.);
#6833=ORIENTED_EDGE('',*,*,#4870,.F.);
#6834=ORIENTED_EDGE('',*,*,#4854,.F.);
#6835=ORIENTED_EDGE('',*,*,#4870,.T.);
#6836=ORIENTED_EDGE('',*,*,#4871,.F.);
#6837=ORIENTED_EDGE('',*,*,#4872,.F.);
#6838=ORIENTED_EDGE('',*,*,#4855,.F.);
#6839=ORIENTED_EDGE('',*,*,#4467,.T.);
#6840=ORIENTED_EDGE('',*,*,#4857,.T.);
#6841=ORIENTED_EDGE('',*,*,#4844,.F.);
#6842=ORIENTED_EDGE('',*,*,#4872,.T.);
#6843=ORIENTED_EDGE('',*,*,#4873,.F.);
#6844=ORIENTED_EDGE('',*,*,#4842,.T.);
#6845=ORIENTED_EDGE('',*,*,#4573,.T.);
#6846=ORIENTED_EDGE('',*,*,#4517,.T.);
#6847=ORIENTED_EDGE('',*,*,#4873,.T.);
#6848=ORIENTED_EDGE('',*,*,#4871,.T.);
#6849=ORIENTED_EDGE('',*,*,#4869,.T.);
#6850=ORIENTED_EDGE('',*,*,#4867,.T.);
#6851=ORIENTED_EDGE('',*,*,#4865,.T.);
#6852=ORIENTED_EDGE('',*,*,#4863,.T.);
#6853=ORIENTED_EDGE('',*,*,#4861,.T.);
#6854=ORIENTED_EDGE('',*,*,#4826,.T.);
#6855=ORIENTED_EDGE('',*,*,#4831,.T.);
#6856=ORIENTED_EDGE('',*,*,#4835,.T.);
#6857=ORIENTED_EDGE('',*,*,#4837,.T.);
#6858=ORIENTED_EDGE('',*,*,#4839,.T.);
#6859=ORIENTED_EDGE('',*,*,#4841,.T.);
#6860=ORIENTED_EDGE('',*,*,#4843,.T.);
#6861=ORIENTED_EDGE('',*,*,#4874,.F.);
#6862=ORIENTED_EDGE('',*,*,#4875,.T.);
#6863=ORIENTED_EDGE('',*,*,#4876,.T.);
#6864=ORIENTED_EDGE('',*,*,#4877,.F.);
#6865=ORIENTED_EDGE('',*,*,#4878,.F.);
#6866=ORIENTED_EDGE('',*,*,#4879,.T.);
#6867=ORIENTED_EDGE('',*,*,#4880,.T.);
#6868=ORIENTED_EDGE('',*,*,#4875,.F.);
#6869=ORIENTED_EDGE('',*,*,#4881,.F.);
#6870=ORIENTED_EDGE('',*,*,#4882,.T.);
#6871=ORIENTED_EDGE('',*,*,#4883,.T.);
#6872=ORIENTED_EDGE('',*,*,#4879,.F.);
#6873=ORIENTED_EDGE('',*,*,#4884,.F.);
#6874=ORIENTED_EDGE('',*,*,#4885,.T.);
#6875=ORIENTED_EDGE('',*,*,#4886,.T.);
#6876=ORIENTED_EDGE('',*,*,#4882,.F.);
#6877=ORIENTED_EDGE('',*,*,#4887,.F.);
#6878=ORIENTED_EDGE('',*,*,#4888,.T.);
#6879=ORIENTED_EDGE('',*,*,#4889,.T.);
#6880=ORIENTED_EDGE('',*,*,#4885,.F.);
#6881=ORIENTED_EDGE('',*,*,#4890,.F.);
#6882=ORIENTED_EDGE('',*,*,#4877,.T.);
#6883=ORIENTED_EDGE('',*,*,#4891,.T.);
#6884=ORIENTED_EDGE('',*,*,#4888,.F.);
#6885=ORIENTED_EDGE('',*,*,#4891,.F.);
#6886=ORIENTED_EDGE('',*,*,#4876,.F.);
#6887=ORIENTED_EDGE('',*,*,#4880,.F.);
#6888=ORIENTED_EDGE('',*,*,#4883,.F.);
#6889=ORIENTED_EDGE('',*,*,#4886,.F.);
#6890=ORIENTED_EDGE('',*,*,#4889,.F.);
#6891=ORIENTED_EDGE('',*,*,#4892,.F.);
#6892=ORIENTED_EDGE('',*,*,#4874,.T.);
#6893=ORIENTED_EDGE('',*,*,#4890,.T.);
#6894=ORIENTED_EDGE('',*,*,#4887,.T.);
#6895=ORIENTED_EDGE('',*,*,#4884,.T.);
#6896=ORIENTED_EDGE('',*,*,#4881,.T.);
#6897=ORIENTED_EDGE('',*,*,#4878,.T.);
#6898=ORIENTED_EDGE('',*,*,#4893,.F.);
#6899=ORIENTED_EDGE('',*,*,#4894,.T.);
#6900=ORIENTED_EDGE('',*,*,#4892,.T.);
#6901=ORIENTED_EDGE('',*,*,#4894,.F.);
#6902=ORIENTED_EDGE('',*,*,#4895,.F.);
#6903=ORIENTED_EDGE('',*,*,#4896,.T.);
#6904=ORIENTED_EDGE('',*,*,#4893,.T.);
#6905=ORIENTED_EDGE('',*,*,#4896,.F.);
#6906=ORIENTED_EDGE('',*,*,#4897,.F.);
#6907=ORIENTED_EDGE('',*,*,#4898,.T.);
#6908=ORIENTED_EDGE('',*,*,#4895,.T.);
#6909=ORIENTED_EDGE('',*,*,#4898,.F.);
#6910=ORIENTED_EDGE('',*,*,#4897,.T.);
#6911=CYLINDRICAL_SURFACE('',#7484,0.21);
#6912=CYLINDRICAL_SURFACE('',#7487,0.21);
#6913=CYLINDRICAL_SURFACE('',#7490,0.21);
#6914=CYLINDRICAL_SURFACE('',#7493,0.21);
#6915=CYLINDRICAL_SURFACE('',#7503,0.6);
#6916=CYLINDRICAL_SURFACE('',#7509,0.6);
#6917=CYLINDRICAL_SURFACE('',#7517,0.525);
#6918=CYLINDRICAL_SURFACE('',#7519,0.525);
#6919=CYLINDRICAL_SURFACE('',#7529,0.225);
#6920=CYLINDRICAL_SURFACE('',#7532,0.165);
#6921=CYLINDRICAL_SURFACE('',#7534,0.275);
#6922=CYLINDRICAL_SURFACE('',#7536,0.275);
#6923=CYLINDRICAL_SURFACE('',#7538,0.6);
#6924=CYLINDRICAL_SURFACE('',#7567,0.425);
#6925=CYLINDRICAL_SURFACE('',#7575,0.24505);
#6926=CYLINDRICAL_SURFACE('',#7581,0.35);
#6927=CYLINDRICAL_SURFACE('',#7589,0.1954);
#6928=CYLINDRICAL_SURFACE('',#7603,0.2117);
#6929=CYLINDRICAL_SURFACE('',#7609,1.1);
#6930=CYLINDRICAL_SURFACE('',#7615,0.6);
#6931=CYLINDRICAL_SURFACE('',#7618,0.21);
#6932=CYLINDRICAL_SURFACE('',#7619,0.6);
#6933=CYLINDRICAL_SURFACE('',#7732,1.37);
#6934=CYLINDRICAL_SURFACE('',#7736,0.21);
#6935=CYLINDRICAL_SURFACE('',#7737,0.6);
#6936=CYLINDRICAL_SURFACE('',#7850,1.37);
#6937=CYLINDRICAL_SURFACE('',#7861,0.817);
#6938=CYLINDRICAL_SURFACE('',#7863,0.817);
#6939=CYLINDRICAL_SURFACE('',#7865,0.817);
#6940=CYLINDRICAL_SURFACE('',#7867,0.817);
#6941=CYLINDRICAL_SURFACE('',#7869,0.817);
#6942=CYLINDRICAL_SURFACE('',#7871,0.817);
#6943=CYLINDRICAL_SURFACE('',#8021,0.24505);
#6944=ADVANCED_FACE('',(#553),#6911,.F.);
#6945=ADVANCED_FACE('',(#554),#6912,.F.);
#6946=ADVANCED_FACE('',(#555),#6913,.F.);
#6947=ADVANCED_FACE('',(#556),#6914,.F.);
#6948=ADVANCED_FACE('',(#557),#194,.T.);
#6949=ADVANCED_FACE('',(#558),#195,.T.);
#6950=ADVANCED_FACE('',(#559),#196,.T.);
#6951=ADVANCED_FACE('',(#560),#197,.T.);
#6952=ADVANCED_FACE('',(#561,#161,#162,#163,#164),#198,.T.);
#6953=ADVANCED_FACE('',(#562,#165,#166,#167,#168),#199,.F.);
#6954=ADVANCED_FACE('',(#563),#6915,.T.);
#6955=ADVANCED_FACE('',(#564),#200,.T.);
#6956=ADVANCED_FACE('',(#565),#201,.F.);
#6957=ADVANCED_FACE('',(#566),#6916,.T.);
#6958=ADVANCED_FACE('',(#567),#202,.T.);
#6959=ADVANCED_FACE('',(#568),#203,.F.);
#6960=ADVANCED_FACE('',(#569),#204,.F.);
#6961=ADVANCED_FACE('',(#570),#6917,.F.);
#6962=ADVANCED_FACE('',(#571),#6918,.F.);
#6963=ADVANCED_FACE('',(#572),#205,.F.);
#6964=ADVANCED_FACE('',(#573,#169),#206,.T.);
#6965=ADVANCED_FACE('',(#574,#170),#207,.T.);
#6966=ADVANCED_FACE('',(#575,#171),#208,.T.);
#6967=ADVANCED_FACE('',(#576),#6919,.F.);
#6968=ADVANCED_FACE('',(#577),#6920,.F.);
#6969=ADVANCED_FACE('',(#578),#6921,.F.);
#6970=ADVANCED_FACE('',(#579),#6922,.F.);
#6971=ADVANCED_FACE('',(#580),#6923,.F.);
#6972=ADVANCED_FACE('',(#581,#172),#209,.T.);
#6973=ADVANCED_FACE('',(#582),#210,.T.);
#6974=ADVANCED_FACE('',(#583,#173,#174),#211,.T.);
#6975=ADVANCED_FACE('',(#584),#212,.T.);
#6976=ADVANCED_FACE('',(#585,#175),#213,.T.);
#6977=ADVANCED_FACE('',(#586),#214,.T.);
#6978=ADVANCED_FACE('',(#587,#176),#215,.T.);
#6979=ADVANCED_FACE('',(#588),#216,.T.);
#6980=ADVANCED_FACE('',(#589,#177),#217,.T.);
#6981=ADVANCED_FACE('',(#590),#218,.T.);
#6982=ADVANCED_FACE('',(#591,#178),#219,.T.);
#6983=ADVANCED_FACE('',(#592),#220,.F.);
#6984=ADVANCED_FACE('',(#593),#221,.F.);
#6985=ADVANCED_FACE('',(#594),#222,.F.);
#6986=ADVANCED_FACE('',(#595),#223,.F.);
#6987=ADVANCED_FACE('',(#596),#224,.F.);
#6988=ADVANCED_FACE('',(#597),#225,.F.);
#6989=ADVANCED_FACE('',(#598),#226,.F.);
#6990=ADVANCED_FACE('',(#599),#227,.F.);
#6991=ADVANCED_FACE('',(#600),#228,.F.);
#6992=ADVANCED_FACE('',(#601),#229,.T.);
#6993=ADVANCED_FACE('',(#602),#104,.T.);
#6994=ADVANCED_FACE('',(#603),#6924,.T.);
#6995=ADVANCED_FACE('',(#604),#105,.T.);
#6996=ADVANCED_FACE('',(#605,#179),#230,.T.);
#6997=ADVANCED_FACE('',(#606),#106,.T.);
#6998=ADVANCED_FACE('',(#607),#6925,.T.);
#6999=ADVANCED_FACE('',(#608),#231,.T.);
#7000=ADVANCED_FACE('',(#609),#107,.T.);
#7001=ADVANCED_FACE('',(#610),#6926,.T.);
#7002=ADVANCED_FACE('',(#611),#108,.T.);
#7003=ADVANCED_FACE('',(#612,#180),#232,.T.);
#7004=ADVANCED_FACE('',(#613),#109,.T.);
#7005=ADVANCED_FACE('',(#614),#6927,.T.);
#7006=ADVANCED_FACE('',(#615),#110,.T.);
#7007=ADVANCED_FACE('',(#616),#233,.T.);
#7008=ADVANCED_FACE('',(#617),#234,.F.);
#7009=ADVANCED_FACE('',(#618),#235,.F.);
#7010=ADVANCED_FACE('',(#619),#236,.F.);
#7011=ADVANCED_FACE('',(#620),#237,.F.);
#7012=ADVANCED_FACE('',(#621),#238,.F.);
#7013=ADVANCED_FACE('',(#622),#239,.F.);
#7014=ADVANCED_FACE('',(#623),#240,.F.);
#7015=ADVANCED_FACE('',(#624),#241,.F.);
#7016=ADVANCED_FACE('',(#625),#6928,.F.);
#7017=ADVANCED_FACE('',(#626,#181),#242,.T.);
#7018=ADVANCED_FACE('',(#627),#111,.T.);
#7019=ADVANCED_FACE('',(#628,#182),#6929,.T.);
#7020=ADVANCED_FACE('',(#629),#112,.T.);
#7021=ADVANCED_FACE('',(#630,#183),#243,.T.);
#7022=ADVANCED_FACE('',(#631,#184),#6930,.F.);
#7023=ADVANCED_FACE('',(#632),#6931,.F.);
#7024=ADVANCED_FACE('',(#633,#185),#6932,.F.);
#7025=ADVANCED_FACE('',(#634),#244,.T.);
#7026=ADVANCED_FACE('',(#635),#245,.T.);
#7027=ADVANCED_FACE('',(#636),#246,.T.);
#7028=ADVANCED_FACE('',(#637),#247,.T.);
#7029=ADVANCED_FACE('',(#638),#248,.T.);
#7030=ADVANCED_FACE('',(#639),#249,.T.);
#7031=ADVANCED_FACE('',(#640),#250,.T.);
#7032=ADVANCED_FACE('',(#641),#251,.T.);
#7033=ADVANCED_FACE('',(#642),#252,.T.);
#7034=ADVANCED_FACE('',(#643),#253,.T.);
#7035=ADVANCED_FACE('',(#644),#254,.T.);
#7036=ADVANCED_FACE('',(#645),#255,.T.);
#7037=ADVANCED_FACE('',(#646),#256,.T.);
#7038=ADVANCED_FACE('',(#647),#257,.T.);
#7039=ADVANCED_FACE('',(#648),#258,.T.);
#7040=ADVANCED_FACE('',(#649),#259,.T.);
#7041=ADVANCED_FACE('',(#650),#260,.T.);
#7042=ADVANCED_FACE('',(#651),#261,.T.);
#7043=ADVANCED_FACE('',(#652),#262,.T.);
#7044=ADVANCED_FACE('',(#653),#263,.T.);
#7045=ADVANCED_FACE('',(#654),#264,.T.);
#7046=ADVANCED_FACE('',(#655),#265,.T.);
#7047=ADVANCED_FACE('',(#656),#266,.T.);
#7048=ADVANCED_FACE('',(#657),#267,.T.);
#7049=ADVANCED_FACE('',(#658),#268,.T.);
#7050=ADVANCED_FACE('',(#659),#269,.T.);
#7051=ADVANCED_FACE('',(#660),#270,.T.);
#7052=ADVANCED_FACE('',(#661,#186),#271,.T.);
#7053=ADVANCED_FACE('',(#662),#272,.T.);
#7054=ADVANCED_FACE('',(#663),#273,.T.);
#7055=ADVANCED_FACE('',(#664),#274,.T.);
#7056=ADVANCED_FACE('',(#665),#275,.T.);
#7057=ADVANCED_FACE('',(#666),#276,.T.);
#7058=ADVANCED_FACE('',(#667),#277,.T.);
#7059=ADVANCED_FACE('',(#668),#278,.T.);
#7060=ADVANCED_FACE('',(#669),#279,.T.);
#7061=ADVANCED_FACE('',(#670),#280,.T.);
#7062=ADVANCED_FACE('',(#671),#281,.T.);
#7063=ADVANCED_FACE('',(#672),#282,.T.);
#7064=ADVANCED_FACE('',(#673),#283,.T.);
#7065=ADVANCED_FACE('',(#674),#284,.T.);
#7066=ADVANCED_FACE('',(#675),#285,.T.);
#7067=ADVANCED_FACE('',(#676),#286,.T.);
#7068=ADVANCED_FACE('',(#677),#287,.T.);
#7069=ADVANCED_FACE('',(#678),#288,.T.);
#7070=ADVANCED_FACE('',(#679),#289,.T.);
#7071=ADVANCED_FACE('',(#680),#290,.T.);
#7072=ADVANCED_FACE('',(#681),#291,.T.);
#7073=ADVANCED_FACE('',(#682),#292,.T.);
#7074=ADVANCED_FACE('',(#683),#293,.T.);
#7075=ADVANCED_FACE('',(#684),#294,.T.);
#7076=ADVANCED_FACE('',(#685),#295,.T.);
#7077=ADVANCED_FACE('',(#686),#296,.T.);
#7078=ADVANCED_FACE('',(#687),#297,.T.);
#7079=ADVANCED_FACE('',(#688),#298,.T.);
#7080=ADVANCED_FACE('',(#689),#299,.T.);
#7081=ADVANCED_FACE('',(#690),#300,.T.);
#7082=ADVANCED_FACE('',(#691),#301,.T.);
#7083=ADVANCED_FACE('',(#692),#302,.T.);
#7084=ADVANCED_FACE('',(#693),#303,.T.);
#7085=ADVANCED_FACE('',(#694),#304,.T.);
#7086=ADVANCED_FACE('',(#695),#305,.T.);
#7087=ADVANCED_FACE('',(#696),#306,.T.);
#7088=ADVANCED_FACE('',(#697),#307,.T.);
#7089=ADVANCED_FACE('',(#698),#308,.T.);
#7090=ADVANCED_FACE('',(#699),#309,.T.);
#7091=ADVANCED_FACE('',(#700),#310,.T.);
#7092=ADVANCED_FACE('',(#701),#311,.T.);
#7093=ADVANCED_FACE('',(#702),#312,.T.);
#7094=ADVANCED_FACE('',(#703),#313,.T.);
#7095=ADVANCED_FACE('',(#704),#314,.T.);
#7096=ADVANCED_FACE('',(#705),#315,.T.);
#7097=ADVANCED_FACE('',(#706),#316,.T.);
#7098=ADVANCED_FACE('',(#707),#317,.T.);
#7099=ADVANCED_FACE('',(#708),#318,.T.);
#7100=ADVANCED_FACE('',(#709),#319,.T.);
#7101=ADVANCED_FACE('',(#710),#320,.T.);
#7102=ADVANCED_FACE('',(#711),#321,.T.);
#7103=ADVANCED_FACE('',(#712),#322,.T.);
#7104=ADVANCED_FACE('',(#713),#323,.T.);
#7105=ADVANCED_FACE('',(#714),#324,.T.);
#7106=ADVANCED_FACE('',(#715),#325,.T.);
#7107=ADVANCED_FACE('',(#716,#187),#6933,.T.);
#7108=ADVANCED_FACE('',(#717,#188),#326,.F.);
#7109=ADVANCED_FACE('',(#718),#6934,.F.);
#7110=ADVANCED_FACE('',(#719,#189),#6935,.F.);
#7111=ADVANCED_FACE('',(#720),#327,.T.);
#7112=ADVANCED_FACE('',(#721),#328,.T.);
#7113=ADVANCED_FACE('',(#722),#329,.T.);
#7114=ADVANCED_FACE('',(#723),#330,.T.);
#7115=ADVANCED_FACE('',(#724),#331,.T.);
#7116=ADVANCED_FACE('',(#725),#332,.T.);
#7117=ADVANCED_FACE('',(#726),#333,.T.);
#7118=ADVANCED_FACE('',(#727),#334,.T.);
#7119=ADVANCED_FACE('',(#728),#335,.T.);
#7120=ADVANCED_FACE('',(#729),#336,.T.);
#7121=ADVANCED_FACE('',(#730),#337,.T.);
#7122=ADVANCED_FACE('',(#731),#338,.T.);
#7123=ADVANCED_FACE('',(#732),#339,.T.);
#7124=ADVANCED_FACE('',(#733),#340,.T.);
#7125=ADVANCED_FACE('',(#734),#341,.T.);
#7126=ADVANCED_FACE('',(#735),#342,.T.);
#7127=ADVANCED_FACE('',(#736),#343,.T.);
#7128=ADVANCED_FACE('',(#737),#344,.T.);
#7129=ADVANCED_FACE('',(#738),#345,.F.);
#7130=ADVANCED_FACE('',(#739),#346,.F.);
#7131=ADVANCED_FACE('',(#740),#347,.F.);
#7132=ADVANCED_FACE('',(#741),#348,.F.);
#7133=ADVANCED_FACE('',(#742),#349,.F.);
#7134=ADVANCED_FACE('',(#743),#350,.F.);
#7135=ADVANCED_FACE('',(#744),#351,.F.);
#7136=ADVANCED_FACE('',(#745,#190),#352,.F.);
#7137=ADVANCED_FACE('',(#746),#353,.F.);
#7138=ADVANCED_FACE('',(#747),#354,.F.);
#7139=ADVANCED_FACE('',(#748),#355,.T.);
#7140=ADVANCED_FACE('',(#749),#356,.T.);
#7141=ADVANCED_FACE('',(#750),#357,.T.);
#7142=ADVANCED_FACE('',(#751),#358,.T.);
#7143=ADVANCED_FACE('',(#752),#359,.T.);
#7144=ADVANCED_FACE('',(#753),#360,.T.);
#7145=ADVANCED_FACE('',(#754),#361,.T.);
#7146=ADVANCED_FACE('',(#755),#362,.T.);
#7147=ADVANCED_FACE('',(#756),#363,.T.);
#7148=ADVANCED_FACE('',(#757),#364,.T.);
#7149=ADVANCED_FACE('',(#758),#365,.T.);
#7150=ADVANCED_FACE('',(#759),#366,.T.);
#7151=ADVANCED_FACE('',(#760),#367,.T.);
#7152=ADVANCED_FACE('',(#761),#368,.T.);
#7153=ADVANCED_FACE('',(#762),#369,.T.);
#7154=ADVANCED_FACE('',(#763),#370,.T.);
#7155=ADVANCED_FACE('',(#764),#371,.T.);
#7156=ADVANCED_FACE('',(#765),#372,.T.);
#7157=ADVANCED_FACE('',(#766),#373,.F.);
#7158=ADVANCED_FACE('',(#767),#374,.F.);
#7159=ADVANCED_FACE('',(#768),#375,.F.);
#7160=ADVANCED_FACE('',(#769),#376,.F.);
#7161=ADVANCED_FACE('',(#770),#377,.F.);
#7162=ADVANCED_FACE('',(#771),#378,.F.);
#7163=ADVANCED_FACE('',(#772),#379,.F.);
#7164=ADVANCED_FACE('',(#773),#380,.F.);
#7165=ADVANCED_FACE('',(#774),#381,.F.);
#7166=ADVANCED_FACE('',(#775),#382,.T.);
#7167=ADVANCED_FACE('',(#776),#383,.T.);
#7168=ADVANCED_FACE('',(#777),#384,.T.);
#7169=ADVANCED_FACE('',(#778),#385,.T.);
#7170=ADVANCED_FACE('',(#779),#386,.T.);
#7171=ADVANCED_FACE('',(#780),#387,.T.);
#7172=ADVANCED_FACE('',(#781),#388,.T.);
#7173=ADVANCED_FACE('',(#782),#389,.T.);
#7174=ADVANCED_FACE('',(#783),#390,.T.);
#7175=ADVANCED_FACE('',(#784),#391,.T.);
#7176=ADVANCED_FACE('',(#785),#392,.T.);
#7177=ADVANCED_FACE('',(#786),#393,.T.);
#7178=ADVANCED_FACE('',(#787),#394,.T.);
#7179=ADVANCED_FACE('',(#788),#395,.T.);
#7180=ADVANCED_FACE('',(#789),#396,.T.);
#7181=ADVANCED_FACE('',(#790),#397,.T.);
#7182=ADVANCED_FACE('',(#791),#398,.T.);
#7183=ADVANCED_FACE('',(#792),#399,.T.);
#7184=ADVANCED_FACE('',(#793),#400,.F.);
#7185=ADVANCED_FACE('',(#794),#401,.F.);
#7186=ADVANCED_FACE('',(#795),#402,.F.);
#7187=ADVANCED_FACE('',(#796),#403,.F.);
#7188=ADVANCED_FACE('',(#797),#404,.F.);
#7189=ADVANCED_FACE('',(#798),#405,.F.);
#7190=ADVANCED_FACE('',(#799),#406,.F.);
#7191=ADVANCED_FACE('',(#800),#407,.F.);
#7192=ADVANCED_FACE('',(#801),#408,.F.);
#7193=ADVANCED_FACE('',(#802,#191),#6936,.T.);
#7194=ADVANCED_FACE('',(#803,#192),#409,.T.);
#7195=ADVANCED_FACE('',(#804),#410,.F.);
#7196=ADVANCED_FACE('',(#805),#6937,.T.);
#7197=ADVANCED_FACE('',(#806),#6938,.T.);
#7198=ADVANCED_FACE('',(#807),#6939,.T.);
#7199=ADVANCED_FACE('',(#808),#6940,.T.);
#7200=ADVANCED_FACE('',(#809),#6941,.T.);
#7201=ADVANCED_FACE('',(#810),#6942,.T.);
#7202=ADVANCED_FACE('',(#811),#411,.T.);
#7203=ADVANCED_FACE('',(#812),#412,.T.);
#7204=ADVANCED_FACE('',(#813),#413,.T.);
#7205=ADVANCED_FACE('',(#814),#414,.T.);
#7206=ADVANCED_FACE('',(#815),#415,.T.);
#7207=ADVANCED_FACE('',(#816),#416,.T.);
#7208=ADVANCED_FACE('',(#817),#417,.T.);
#7209=ADVANCED_FACE('',(#818),#418,.T.);
#7210=ADVANCED_FACE('',(#819),#419,.T.);
#7211=ADVANCED_FACE('',(#820),#420,.T.);
#7212=ADVANCED_FACE('',(#821),#421,.T.);
#7213=ADVANCED_FACE('',(#822),#422,.T.);
#7214=ADVANCED_FACE('',(#823),#423,.T.);
#7215=ADVANCED_FACE('',(#824),#424,.T.);
#7216=ADVANCED_FACE('',(#825),#425,.T.);
#7217=ADVANCED_FACE('',(#826),#426,.T.);
#7218=ADVANCED_FACE('',(#827),#427,.T.);
#7219=ADVANCED_FACE('',(#828),#428,.T.);
#7220=ADVANCED_FACE('',(#829),#429,.T.);
#7221=ADVANCED_FACE('',(#830),#430,.T.);
#7222=ADVANCED_FACE('',(#831),#431,.T.);
#7223=ADVANCED_FACE('',(#832),#432,.T.);
#7224=ADVANCED_FACE('',(#833),#433,.T.);
#7225=ADVANCED_FACE('',(#834),#434,.T.);
#7226=ADVANCED_FACE('',(#835),#435,.T.);
#7227=ADVANCED_FACE('',(#836),#436,.T.);
#7228=ADVANCED_FACE('',(#837),#437,.T.);
#7229=ADVANCED_FACE('',(#838),#438,.T.);
#7230=ADVANCED_FACE('',(#839),#439,.T.);
#7231=ADVANCED_FACE('',(#840),#440,.T.);
#7232=ADVANCED_FACE('',(#841),#441,.T.);
#7233=ADVANCED_FACE('',(#842),#442,.T.);
#7234=ADVANCED_FACE('',(#843),#443,.T.);
#7235=ADVANCED_FACE('',(#844),#444,.T.);
#7236=ADVANCED_FACE('',(#845),#445,.T.);
#7237=ADVANCED_FACE('',(#846),#446,.T.);
#7238=ADVANCED_FACE('',(#847),#447,.T.);
#7239=ADVANCED_FACE('',(#848),#448,.T.);
#7240=ADVANCED_FACE('',(#849),#449,.T.);
#7241=ADVANCED_FACE('',(#850),#450,.T.);
#7242=ADVANCED_FACE('',(#851),#451,.T.);
#7243=ADVANCED_FACE('',(#852),#452,.T.);
#7244=ADVANCED_FACE('',(#853),#453,.T.);
#7245=ADVANCED_FACE('',(#854),#454,.T.);
#7246=ADVANCED_FACE('',(#855),#455,.T.);
#7247=ADVANCED_FACE('',(#856),#456,.T.);
#7248=ADVANCED_FACE('',(#857),#457,.T.);
#7249=ADVANCED_FACE('',(#858),#458,.T.);
#7250=ADVANCED_FACE('',(#859),#459,.T.);
#7251=ADVANCED_FACE('',(#860),#460,.T.);
#7252=ADVANCED_FACE('',(#861),#461,.T.);
#7253=ADVANCED_FACE('',(#862),#462,.T.);
#7254=ADVANCED_FACE('',(#863),#463,.T.);
#7255=ADVANCED_FACE('',(#864),#464,.T.);
#7256=ADVANCED_FACE('',(#865),#465,.T.);
#7257=ADVANCED_FACE('',(#866),#466,.T.);
#7258=ADVANCED_FACE('',(#867),#467,.T.);
#7259=ADVANCED_FACE('',(#868),#468,.T.);
#7260=ADVANCED_FACE('',(#869),#469,.T.);
#7261=ADVANCED_FACE('',(#870),#470,.T.);
#7262=ADVANCED_FACE('',(#871),#471,.T.);
#7263=ADVANCED_FACE('',(#872),#472,.T.);
#7264=ADVANCED_FACE('',(#873),#473,.T.);
#7265=ADVANCED_FACE('',(#874),#474,.T.);
#7266=ADVANCED_FACE('',(#875),#475,.T.);
#7267=ADVANCED_FACE('',(#876),#476,.T.);
#7268=ADVANCED_FACE('',(#877),#477,.T.);
#7269=ADVANCED_FACE('',(#878),#478,.T.);
#7270=ADVANCED_FACE('',(#879),#479,.T.);
#7271=ADVANCED_FACE('',(#880),#480,.T.);
#7272=ADVANCED_FACE('',(#881),#481,.T.);
#7273=ADVANCED_FACE('',(#882),#482,.T.);
#7274=ADVANCED_FACE('',(#883),#483,.T.);
#7275=ADVANCED_FACE('',(#884),#484,.T.);
#7276=ADVANCED_FACE('',(#885),#485,.T.);
#7277=ADVANCED_FACE('',(#886),#486,.T.);
#7278=ADVANCED_FACE('',(#887),#487,.T.);
#7279=ADVANCED_FACE('',(#888),#488,.T.);
#7280=ADVANCED_FACE('',(#889),#489,.T.);
#7281=ADVANCED_FACE('',(#890),#490,.T.);
#7282=ADVANCED_FACE('',(#891),#491,.T.);
#7283=ADVANCED_FACE('',(#892),#492,.T.);
#7284=ADVANCED_FACE('',(#893),#493,.T.);
#7285=ADVANCED_FACE('',(#894),#494,.T.);
#7286=ADVANCED_FACE('',(#895),#495,.T.);
#7287=ADVANCED_FACE('',(#896),#496,.T.);
#7288=ADVANCED_FACE('',(#897),#497,.T.);
#7289=ADVANCED_FACE('',(#898),#498,.T.);
#7290=ADVANCED_FACE('',(#899),#499,.T.);
#7291=ADVANCED_FACE('',(#900),#500,.T.);
#7292=ADVANCED_FACE('',(#901),#501,.T.);
#7293=ADVANCED_FACE('',(#902),#502,.T.);
#7294=ADVANCED_FACE('',(#903),#503,.T.);
#7295=ADVANCED_FACE('',(#904),#504,.T.);
#7296=ADVANCED_FACE('',(#905),#505,.T.);
#7297=ADVANCED_FACE('',(#906),#506,.T.);
#7298=ADVANCED_FACE('',(#907),#507,.T.);
#7299=ADVANCED_FACE('',(#908),#508,.T.);
#7300=ADVANCED_FACE('',(#909),#509,.T.);
#7301=ADVANCED_FACE('',(#910),#510,.T.);
#7302=ADVANCED_FACE('',(#911),#511,.T.);
#7303=ADVANCED_FACE('',(#912),#512,.T.);
#7304=ADVANCED_FACE('',(#913),#513,.T.);
#7305=ADVANCED_FACE('',(#914),#514,.T.);
#7306=ADVANCED_FACE('',(#915),#515,.T.);
#7307=ADVANCED_FACE('',(#916),#516,.T.);
#7308=ADVANCED_FACE('',(#917),#517,.T.);
#7309=ADVANCED_FACE('',(#918),#518,.T.);
#7310=ADVANCED_FACE('',(#919),#519,.T.);
#7311=ADVANCED_FACE('',(#920),#520,.T.);
#7312=ADVANCED_FACE('',(#921),#521,.T.);
#7313=ADVANCED_FACE('',(#922),#522,.T.);
#7314=ADVANCED_FACE('',(#923),#523,.T.);
#7315=ADVANCED_FACE('',(#924),#524,.T.);
#7316=ADVANCED_FACE('',(#925),#525,.T.);
#7317=ADVANCED_FACE('',(#926),#526,.T.);
#7318=ADVANCED_FACE('',(#927),#527,.T.);
#7319=ADVANCED_FACE('',(#928),#528,.T.);
#7320=ADVANCED_FACE('',(#929),#529,.T.);
#7321=ADVANCED_FACE('',(#930),#530,.T.);
#7322=ADVANCED_FACE('',(#931),#531,.T.);
#7323=ADVANCED_FACE('',(#932),#532,.T.);
#7324=ADVANCED_FACE('',(#933),#533,.T.);
#7325=ADVANCED_FACE('',(#934),#534,.T.);
#7326=ADVANCED_FACE('',(#935),#535,.T.);
#7327=ADVANCED_FACE('',(#936),#536,.T.);
#7328=ADVANCED_FACE('',(#937),#537,.T.);
#7329=ADVANCED_FACE('',(#938),#538,.T.);
#7330=ADVANCED_FACE('',(#939),#539,.T.);
#7331=ADVANCED_FACE('',(#940),#540,.T.);
#7332=ADVANCED_FACE('',(#941),#541,.T.);
#7333=ADVANCED_FACE('',(#942),#542,.T.);
#7334=ADVANCED_FACE('',(#943),#543,.T.);
#7335=ADVANCED_FACE('',(#944),#544,.F.);
#7336=ADVANCED_FACE('',(#945),#545,.F.);
#7337=ADVANCED_FACE('',(#946),#546,.F.);
#7338=ADVANCED_FACE('',(#947),#547,.F.);
#7339=ADVANCED_FACE('',(#948),#548,.F.);
#7340=ADVANCED_FACE('',(#949),#549,.F.);
#7341=ADVANCED_FACE('',(#950),#550,.F.);
#7342=ADVANCED_FACE('',(#951,#193),#551,.T.);
#7343=ADVANCED_FACE('',(#952),#113,.T.);
#7344=ADVANCED_FACE('',(#953),#6943,.T.);
#7345=ADVANCED_FACE('',(#954),#114,.T.);
#7346=ADVANCED_FACE('',(#955),#552,.T.);
#7347=CLOSED_SHELL('',(#6944,#6945,#6946,#6947,#6948,#6949,#6950,#6951,
#6952,#6953));
#7348=CLOSED_SHELL('',(#6954,#6955,#6956));
#7349=CLOSED_SHELL('',(#6957,#6958,#6959));
#7350=CLOSED_SHELL('',(#6960,#6961,#6962,#6963,#6964,#6965,#6966,#6967,
#6968,#6969,#6970,#6971,#6972,#6973,#6974,#6975,#6976,#6977,#6978,#6979,
#6980,#6981,#6982));
#7351=CLOSED_SHELL('',(#6983,#6984,#6985,#6986,#6987,#6988,#6989,#6990));
#7352=CLOSED_SHELL('',(#6991,#6992,#6993,#6994,#6995,#6996,#6997,#6998));
#7353=CLOSED_SHELL('',(#6999,#7000,#7001,#7002,#7003,#7004,#7005,#7006,
#7007));
#7354=CLOSED_SHELL('',(#7008,#7009,#7010,#7011,#7012,#7013,#7014,#7015));
#7355=CLOSED_SHELL('',(#7016,#7017,#7018,#7019,#7020,#7021,#7022));
#7356=CLOSED_SHELL('',(#7023,#7024,#7025,#7026,#7027,#7028,#7029,#7030,
#7031,#7032,#7033,#7034,#7035,#7036,#7037,#7038,#7039,#7040,#7041,#7042,
#7043,#7044,#7045,#7046,#7047,#7048,#7049,#7050,#7051,#7052,#7053,#7054,
#7055,#7056,#7057,#7058,#7059,#7060,#7061,#7062,#7063,#7064,#7065,#7066,
#7067,#7068,#7069,#7070,#7071,#7072,#7073,#7074,#7075,#7076,#7077,#7078,
#7079,#7080,#7081,#7082,#7083,#7084,#7085,#7086,#7087,#7088,#7089,#7090,
#7091,#7092,#7093,#7094,#7095,#7096,#7097,#7098,#7099,#7100,#7101,#7102,
#7103,#7104,#7105,#7106,#7107,#7108));
#7357=CLOSED_SHELL('',(#7109,#7110,#7111,#7112,#7113,#7114,#7115,#7116,
#7117,#7118,#7119,#7120,#7121,#7122,#7123,#7124,#7125,#7126,#7127,#7128,
#7129,#7130,#7131,#7132,#7133,#7134,#7135,#7136,#7137,#7138,#7139,#7140,
#7141,#7142,#7143,#7144,#7145,#7146,#7147,#7148,#7149,#7150,#7151,#7152,
#7153,#7154,#7155,#7156,#7157,#7158,#7159,#7160,#7161,#7162,#7163,#7164,
#7165,#7166,#7167,#7168,#7169,#7170,#7171,#7172,#7173,#7174,#7175,#7176,
#7177,#7178,#7179,#7180,#7181,#7182,#7183,#7184,#7185,#7186,#7187,#7188,
#7189,#7190,#7191,#7192,#7193,#7194));
#7358=CLOSED_SHELL('',(#7195,#7196,#7197,#7198,#7199,#7200,#7201,#7202,
#7203,#7204,#7205,#7206,#7207,#7208,#7209,#7210,#7211,#7212,#7213,#7214,
#7215,#7216,#7217,#7218,#7219,#7220,#7221,#7222,#7223,#7224,#7225,#7226,
#7227,#7228,#7229,#7230,#7231,#7232,#7233,#7234,#7235,#7236,#7237,#7238,
#7239,#7240,#7241,#7242,#7243,#7244,#7245,#7246,#7247,#7248,#7249,#7250,
#7251,#7252,#7253,#7254,#7255,#7256,#7257,#7258,#7259,#7260,#7261,#7262,
#7263,#7264,#7265,#7266,#7267,#7268,#7269,#7270,#7271,#7272,#7273,#7274,
#7275,#7276,#7277,#7278,#7279,#7280,#7281,#7282,#7283,#7284,#7285,#7286,
#7287,#7288,#7289,#7290,#7291,#7292,#7293,#7294,#7295,#7296,#7297,#7298,
#7299,#7300,#7301,#7302,#7303,#7304,#7305,#7306,#7307,#7308,#7309,#7310,
#7311,#7312,#7313,#7314,#7315,#7316,#7317,#7318,#7319,#7320,#7321,#7322,
#7323,#7324,#7325,#7326,#7327,#7328,#7329,#7330,#7331,#7332,#7333,#7334));
#7359=CLOSED_SHELL('',(#7335,#7336,#7337,#7338,#7339,#7340,#7341,#7342,
#7343,#7344,#7345,#7346));
#7360=DERIVED_UNIT_ELEMENT(#7382,1.);
#7361=DERIVED_UNIT_ELEMENT(#12345,-3.);
#7362=DERIVED_UNIT_ELEMENT(#7382,1.);
#7363=DERIVED_UNIT_ELEMENT(#12345,-3.);
#7364=DERIVED_UNIT_ELEMENT(#7382,1.);
#7365=DERIVED_UNIT_ELEMENT(#12345,-3.);
#7366=DERIVED_UNIT_ELEMENT(#7382,1.);
#7367=DERIVED_UNIT_ELEMENT(#12345,-3.);
#7368=DERIVED_UNIT_ELEMENT(#7382,1.);
#7369=DERIVED_UNIT_ELEMENT(#12345,-3.);
#7370=DERIVED_UNIT_ELEMENT(#7382,1.);
#7371=DERIVED_UNIT_ELEMENT(#12345,-3.);
#7372=DERIVED_UNIT_ELEMENT(#7382,1.);
#7373=DERIVED_UNIT_ELEMENT(#12345,-3.);
#7374=DERIVED_UNIT_ELEMENT(#7382,1.);
#7375=DERIVED_UNIT_ELEMENT(#12345,-3.);
#7376=DERIVED_UNIT_ELEMENT(#7382,1.);
#7377=DERIVED_UNIT_ELEMENT(#12345,-3.);
#7378=DERIVED_UNIT_ELEMENT(#7382,1.);
#7379=DERIVED_UNIT_ELEMENT(#12345,-3.);
#7380=DERIVED_UNIT_ELEMENT(#7382,1.);
#7381=DERIVED_UNIT_ELEMENT(#12345,-3.);
#7382=(
MASS_UNIT()
NAMED_UNIT(*)
SI_UNIT(.KILO.,.GRAM.)
);
#7383=DERIVED_UNIT((#7360,#7361));
#7384=DERIVED_UNIT((#7362,#7363));
#7385=DERIVED_UNIT((#7364,#7365));
#7386=DERIVED_UNIT((#7366,#7367));
#7387=DERIVED_UNIT((#7368,#7369));
#7388=DERIVED_UNIT((#7370,#7371));
#7389=DERIVED_UNIT((#7372,#7373));
#7390=DERIVED_UNIT((#7374,#7375));
#7391=DERIVED_UNIT((#7376,#7377));
#7392=DERIVED_UNIT((#7378,#7379));
#7393=DERIVED_UNIT((#7380,#7381));
#7394=MEASURE_REPRESENTATION_ITEM('density measure',
POSITIVE_RATIO_MEASURE(7850.),#7383);
#7395=MEASURE_REPRESENTATION_ITEM('density measure',
POSITIVE_RATIO_MEASURE(7850.),#7384);
#7396=MEASURE_REPRESENTATION_ITEM('density measure',
POSITIVE_RATIO_MEASURE(7850.),#7385);
#7397=MEASURE_REPRESENTATION_ITEM('density measure',
POSITIVE_RATIO_MEASURE(7850.),#7386);
#7398=MEASURE_REPRESENTATION_ITEM('density measure',
POSITIVE_RATIO_MEASURE(7850.),#7387);
#7399=MEASURE_REPRESENTATION_ITEM('density measure',
POSITIVE_RATIO_MEASURE(7850.),#7388);
#7400=MEASURE_REPRESENTATION_ITEM('density measure',
POSITIVE_RATIO_MEASURE(7850.),#7389);
#7401=MEASURE_REPRESENTATION_ITEM('density measure',
POSITIVE_RATIO_MEASURE(7850.),#7390);
#7402=MEASURE_REPRESENTATION_ITEM('density measure',
POSITIVE_RATIO_MEASURE(7850.),#7391);
#7403=MEASURE_REPRESENTATION_ITEM('density measure',
POSITIVE_RATIO_MEASURE(7850.),#7392);
#7404=MEASURE_REPRESENTATION_ITEM('density measure',
POSITIVE_RATIO_MEASURE(7850.),#7393);
#7405=PROPERTY_DEFINITION_REPRESENTATION(#7460,#7427);
#7406=PROPERTY_DEFINITION_REPRESENTATION(#7461,#7428);
#7407=PROPERTY_DEFINITION_REPRESENTATION(#7462,#7429);
#7408=PROPERTY_DEFINITION_REPRESENTATION(#7463,#7430);
#7409=PROPERTY_DEFINITION_REPRESENTATION(#7464,#7431);
#7410=PROPERTY_DEFINITION_REPRESENTATION(#7465,#7432);
#7411=PROPERTY_DEFINITION_REPRESENTATION(#7466,#7433);
#7412=PROPERTY_DEFINITION_REPRESENTATION(#7467,#7434);
#7413=PROPERTY_DEFINITION_REPRESENTATION(#7468,#7435);
#7414=PROPERTY_DEFINITION_REPRESENTATION(#7469,#7436);
#7415=PROPERTY_DEFINITION_REPRESENTATION(#7470,#7437);
#7416=PROPERTY_DEFINITION_REPRESENTATION(#7471,#7438);
#7417=PROPERTY_DEFINITION_REPRESENTATION(#7472,#7439);
#7418=PROPERTY_DEFINITION_REPRESENTATION(#7473,#7440);
#7419=PROPERTY_DEFINITION_REPRESENTATION(#7474,#7441);
#7420=PROPERTY_DEFINITION_REPRESENTATION(#7475,#7442);
#7421=PROPERTY_DEFINITION_REPRESENTATION(#7476,#7443);
#7422=PROPERTY_DEFINITION_REPRESENTATION(#7477,#7444);
#7423=PROPERTY_DEFINITION_REPRESENTATION(#7478,#7445);
#7424=PROPERTY_DEFINITION_REPRESENTATION(#7479,#7446);
#7425=PROPERTY_DEFINITION_REPRESENTATION(#7480,#7447);
#7426=PROPERTY_DEFINITION_REPRESENTATION(#7481,#7448);
#7427=REPRESENTATION('material name',(#7449),#12331);
#7428=REPRESENTATION('density',(#7394),#12331);
#7429=REPRESENTATION('material name',(#7450),#12332);
#7430=REPRESENTATION('density',(#7395),#12332);
#7431=REPRESENTATION('material name',(#7451),#12333);
#7432=REPRESENTATION('density',(#7396),#12333);
#7433=REPRESENTATION('material name',(#7452),#12334);
#7434=REPRESENTATION('density',(#7397),#12334);
#7435=REPRESENTATION('material name',(#7453),#12335);
#7436=REPRESENTATION('density',(#7398),#12335);
#7437=REPRESENTATION('material name',(#7454),#12336);
#7438=REPRESENTATION('density',(#7399),#12336);
#7439=REPRESENTATION('material name',(#7455),#12337);
#7440=REPRESENTATION('density',(#7400),#12337);
#7441=REPRESENTATION('material name',(#7456),#12339);
#7442=REPRESENTATION('density',(#7401),#12339);
#7443=REPRESENTATION('material name',(#7457),#12340);
#7444=REPRESENTATION('density',(#7402),#12340);
#7445=REPRESENTATION('material name',(#7458),#12341);
#7446=REPRESENTATION('density',(#7403),#12341);
#7447=REPRESENTATION('material name',(#7459),#12342);
#7448=REPRESENTATION('density',(#7404),#12342);
#7449=DESCRIPTIVE_REPRESENTATION_ITEM('Steel','Steel');
#7450=DESCRIPTIVE_REPRESENTATION_ITEM('Steel','Steel');
#7451=DESCRIPTIVE_REPRESENTATION_ITEM('Steel','Steel');
#7452=DESCRIPTIVE_REPRESENTATION_ITEM('Steel','Steel');
#7453=DESCRIPTIVE_REPRESENTATION_ITEM('Steel','Steel');
#7454=DESCRIPTIVE_REPRESENTATION_ITEM('Steel','Steel');
#7455=DESCRIPTIVE_REPRESENTATION_ITEM('Steel','Steel');
#7456=DESCRIPTIVE_REPRESENTATION_ITEM('Steel','Steel');
#7457=DESCRIPTIVE_REPRESENTATION_ITEM('Steel','Steel');
#7458=DESCRIPTIVE_REPRESENTATION_ITEM('Steel','Steel');
#7459=DESCRIPTIVE_REPRESENTATION_ITEM('Steel','Steel');
#7460=PROPERTY_DEFINITION('material property','material name',#12410);
#7461=PROPERTY_DEFINITION('material property','density of part',#12410);
#7462=PROPERTY_DEFINITION('material property','material name',#12411);
#7463=PROPERTY_DEFINITION('material property','density of part',#12411);
#7464=PROPERTY_DEFINITION('material property','material name',#12412);
#7465=PROPERTY_DEFINITION('material property','density of part',#12412);
#7466=PROPERTY_DEFINITION('material property','material name',#12413);
#7467=PROPERTY_DEFINITION('material property','density of part',#12413);
#7468=PROPERTY_DEFINITION('material property','material name',#12414);
#7469=PROPERTY_DEFINITION('material property','density of part',#12414);
#7470=PROPERTY_DEFINITION('material property','material name',#12415);
#7471=PROPERTY_DEFINITION('material property','density of part',#12415);
#7472=PROPERTY_DEFINITION('material property','material name',#12416);
#7473=PROPERTY_DEFINITION('material property','density of part',#12416);
#7474=PROPERTY_DEFINITION('material property','material name',#12418);
#7475=PROPERTY_DEFINITION('material property','density of part',#12418);
#7476=PROPERTY_DEFINITION('material property','material name',#12419);
#7477=PROPERTY_DEFINITION('material property','density of part',#12419);
#7478=PROPERTY_DEFINITION('material property','material name',#12420);
#7479=PROPERTY_DEFINITION('material property','density of part',#12420);
#7480=PROPERTY_DEFINITION('material property','material name',#12421);
#7481=PROPERTY_DEFINITION('material property','density of part',#12421);
#7482=AXIS2_PLACEMENT_3D('',#10040,#8044,#8045);
#7483=AXIS2_PLACEMENT_3D('',#10041,#8046,#8047);
#7484=AXIS2_PLACEMENT_3D('',#10042,#8048,#8049);
#7485=AXIS2_PLACEMENT_3D('',#10044,#8050,#8051);
#7486=AXIS2_PLACEMENT_3D('',#10047,#8053,#8054);
#7487=AXIS2_PLACEMENT_3D('',#10048,#8055,#8056);
#7488=AXIS2_PLACEMENT_3D('',#10050,#8057,#8058);
#7489=AXIS2_PLACEMENT_3D('',#10053,#8060,#8061);
#7490=AXIS2_PLACEMENT_3D('',#10054,#8062,#8063);
#7491=AXIS2_PLACEMENT_3D('',#10056,#8064,#8065);
#7492=AXIS2_PLACEMENT_3D('',#10059,#8067,#8068);
#7493=AXIS2_PLACEMENT_3D('',#10060,#8069,#8070);
#7494=AXIS2_PLACEMENT_3D('',#10062,#8071,#8072);
#7495=AXIS2_PLACEMENT_3D('',#10065,#8074,#8075);
#7496=AXIS2_PLACEMENT_3D('',#10066,#8076,#8077);
#7497=AXIS2_PLACEMENT_3D('',#10075,#8082,#8083);
#7498=AXIS2_PLACEMENT_3D('',#10081,#8087,#8088);
#7499=AXIS2_PLACEMENT_3D('',#10087,#8092,#8093);
#7500=AXIS2_PLACEMENT_3D('',#10090,#8096,#8097);
#7501=AXIS2_PLACEMENT_3D('',#10091,#8098,#8099);
#7502=AXIS2_PLACEMENT_3D('',#10092,#8100,#8101);
#7503=AXIS2_PLACEMENT_3D('',#10093,#8102,#8103);
#7504=AXIS2_PLACEMENT_3D('',#10095,#8104,#8105);
#7505=AXIS2_PLACEMENT_3D('',#10098,#8107,#8108);
#7506=AXIS2_PLACEMENT_3D('',#10099,#8109,#8110);
#7507=AXIS2_PLACEMENT_3D('',#10100,#8111,#8112);
#7508=AXIS2_PLACEMENT_3D('',#10101,#8113,#8114);
#7509=AXIS2_PLACEMENT_3D('',#10102,#8115,#8116);
#7510=AXIS2_PLACEMENT_3D('',#10104,#8117,#8118);
#7511=AXIS2_PLACEMENT_3D('',#10107,#8120,#8121);
#7512=AXIS2_PLACEMENT_3D('',#10108,#8122,#8123);
#7513=AXIS2_PLACEMENT_3D('',#10109,#8124,#8125);
#7514=AXIS2_PLACEMENT_3D('',#10110,#8126,#8127);
#7515=AXIS2_PLACEMENT_3D('',#10111,#8128,#8129);
#7516=AXIS2_PLACEMENT_3D('',#10115,#8131,#8132);
#7517=AXIS2_PLACEMENT_3D('',#10116,#8133,#8134);
#7518=AXIS2_PLACEMENT_3D('',#10120,#8136,#8137);
#7519=AXIS2_PLACEMENT_3D('',#10122,#8139,#8140);
#7520=AXIS2_PLACEMENT_3D('',#10127,#8142,#8143);
#7521=AXIS2_PLACEMENT_3D('',#10130,#8145,#8146);
#7522=AXIS2_PLACEMENT_3D('',#10131,#8147,#8148);
#7523=AXIS2_PLACEMENT_3D('',#10133,#8150,#8151);
#7524=AXIS2_PLACEMENT_3D('',#10144,#8157,#8158);
#7525=AXIS2_PLACEMENT_3D('',#10145,#8159,#8160);
#7526=AXIS2_PLACEMENT_3D('',#10152,#8164,#8165);
#7527=AXIS2_PLACEMENT_3D('',#10153,#8166,#8167);
#7528=AXIS2_PLACEMENT_3D('',#10164,#8173,#8174);
#7529=AXIS2_PLACEMENT_3D('',#10165,#8175,#8176);
#7530=AXIS2_PLACEMENT_3D('',#10167,#8177,#8178);
#7531=AXIS2_PLACEMENT_3D('',#10170,#8180,#8181);
#7532=AXIS2_PLACEMENT_3D('',#10171,#8182,#8183);
#7533=AXIS2_PLACEMENT_3D('',#10174,#8185,#8186);
#7534=AXIS2_PLACEMENT_3D('',#10175,#8187,#8188);
#7535=AXIS2_PLACEMENT_3D('',#10177,#8189,#8190);
#7536=AXIS2_PLACEMENT_3D('',#10179,#8192,#8193);
#7537=AXIS2_PLACEMENT_3D('',#10181,#8194,#8195);
#7538=AXIS2_PLACEMENT_3D('',#10183,#8197,#8198);
#7539=AXIS2_PLACEMENT_3D('',#10185,#8199,#8200);
#7540=AXIS2_PLACEMENT_3D('',#10188,#8202,#8203);
#7541=AXIS2_PLACEMENT_3D('',#10189,#8204,#8205);
#7542=AXIS2_PLACEMENT_3D('',#10206,#8215,#8216);
#7543=AXIS2_PLACEMENT_3D('',#10210,#8219,#8220);
#7544=AXIS2_PLACEMENT_3D('',#10214,#8223,#8224);
#7545=AXIS2_PLACEMENT_3D('',#10216,#8226,#8227);
#7546=AXIS2_PLACEMENT_3D('',#10220,#8230,#8231);
#7547=AXIS2_PLACEMENT_3D('',#10224,#8234,#8235);
#7548=AXIS2_PLACEMENT_3D('',#10228,#8238,#8239);
#7549=AXIS2_PLACEMENT_3D('',#10232,#8242,#8243);
#7550=AXIS2_PLACEMENT_3D('',#10236,#8246,#8247);
#7551=AXIS2_PLACEMENT_3D('',#10238,#8249,#8250);
#7552=AXIS2_PLACEMENT_3D('',#10239,#8251,#8252);
#7553=AXIS2_PLACEMENT_3D('',#10240,#8253,#8254);
#7554=AXIS2_PLACEMENT_3D('',#10249,#8259,#8260);
#7555=AXIS2_PLACEMENT_3D('',#10255,#8264,#8265);
#7556=AXIS2_PLACEMENT_3D('',#10261,#8269,#8270);
#7557=AXIS2_PLACEMENT_3D('',#10267,#8274,#8275);
#7558=AXIS2_PLACEMENT_3D('',#10273,#8279,#8280);
#7559=AXIS2_PLACEMENT_3D('',#10276,#8283,#8284);
#7560=AXIS2_PLACEMENT_3D('',#10277,#8285,#8286);
#7561=AXIS2_PLACEMENT_3D('',#10278,#8287,#8288);
#7562=AXIS2_PLACEMENT_3D('',#10280,#8289,#8290);
#7563=AXIS2_PLACEMENT_3D('',#10281,#8291,#8292);
#7564=AXIS2_PLACEMENT_3D('',#10283,#8293,#8294);
#7565=AXIS2_PLACEMENT_3D('',#10284,#8295,#8296);
#7566=AXIS2_PLACEMENT_3D('',#10286,#8297,#8298);
#7567=AXIS2_PLACEMENT_3D('',#10288,#8300,#8301);
#7568=AXIS2_PLACEMENT_3D('',#10290,#8302,#8303);
#7569=AXIS2_PLACEMENT_3D('',#10292,#8305,#8306);
#7570=AXIS2_PLACEMENT_3D('',#10294,#8307,#8308);
#7571=AXIS2_PLACEMENT_3D('',#10296,#8310,#8311);
#7572=AXIS2_PLACEMENT_3D('',#10298,#8312,#8313);
#7573=AXIS2_PLACEMENT_3D('',#10299,#8314,#8315);
#7574=AXIS2_PLACEMENT_3D('',#10301,#8316,#8317);
#7575=AXIS2_PLACEMENT_3D('',#10303,#8319,#8320);
#7576=AXIS2_PLACEMENT_3D('',#10305,#8322,#8323);
#7577=AXIS2_PLACEMENT_3D('',#10306,#8324,#8325);
#7578=AXIS2_PLACEMENT_3D('',#10308,#8326,#8327);
#7579=AXIS2_PLACEMENT_3D('',#10309,#8328,#8329);
#7580=AXIS2_PLACEMENT_3D('',#10311,#8330,#8331);
#7581=AXIS2_PLACEMENT_3D('',#10313,#8333,#8334);
#7582=AXIS2_PLACEMENT_3D('',#10315,#8335,#8336);
#7583=AXIS2_PLACEMENT_3D('',#10317,#8338,#8339);
#7584=AXIS2_PLACEMENT_3D('',#10319,#8340,#8341);
#7585=AXIS2_PLACEMENT_3D('',#10321,#8343,#8344);
#7586=AXIS2_PLACEMENT_3D('',#10323,#8345,#8346);
#7587=AXIS2_PLACEMENT_3D('',#10324,#8347,#8348);
#7588=AXIS2_PLACEMENT_3D('',#10326,#8349,#8350);
#7589=AXIS2_PLACEMENT_3D('',#10328,#8352,#8353);
#7590=AXIS2_PLACEMENT_3D('',#10330,#8354,#8355);
#7591=AXIS2_PLACEMENT_3D('',#10332,#8357,#8358);
#7592=AXIS2_PLACEMENT_3D('',#10334,#8359,#8360);
#7593=AXIS2_PLACEMENT_3D('',#10336,#8362,#8363);
#7594=AXIS2_PLACEMENT_3D('',#10337,#8364,#8365);
#7595=AXIS2_PLACEMENT_3D('',#10346,#8370,#8371);
#7596=AXIS2_PLACEMENT_3D('',#10352,#8375,#8376);
#7597=AXIS2_PLACEMENT_3D('',#10358,#8380,#8381);
#7598=AXIS2_PLACEMENT_3D('',#10364,#8385,#8386);
#7599=AXIS2_PLACEMENT_3D('',#10370,#8390,#8391);
#7600=AXIS2_PLACEMENT_3D('',#10373,#8394,#8395);
#7601=AXIS2_PLACEMENT_3D('',#10374,#8396,#8397);
#7602=AXIS2_PLACEMENT_3D('',#10375,#8398,#8399);
#7603=AXIS2_PLACEMENT_3D('',#10376,#8400,#8401);
#7604=AXIS2_PLACEMENT_3D('',#10448,#8403,#8404);
#7605=AXIS2_PLACEMENT_3D('',#10450,#8405,#8406);
#7606=AXIS2_PLACEMENT_3D('',#10452,#8407,#8408);
#7607=AXIS2_PLACEMENT_3D('',#10453,#8409,#8410);
#7608=AXIS2_PLACEMENT_3D('',#10455,#8411,#8412);
#7609=AXIS2_PLACEMENT_3D('',#10457,#8414,#8415);
#7610=AXIS2_PLACEMENT_3D('',#10459,#8416,#8417);
#7611=AXIS2_PLACEMENT_3D('',#10461,#8419,#8420);
#7612=AXIS2_PLACEMENT_3D('',#10463,#8421,#8422);
#7613=AXIS2_PLACEMENT_3D('',#10465,#8424,#8425);
#7614=AXIS2_PLACEMENT_3D('',#10467,#8426,#8427);
#7615=AXIS2_PLACEMENT_3D('',#10468,#8428,#8429);
#7616=AXIS2_PLACEMENT_3D('',#10470,#8431,#8432);
#7617=AXIS2_PLACEMENT_3D('',#10471,#8433,#8434);
#7618=AXIS2_PLACEMENT_3D('',#10472,#8435,#8436);
#7619=AXIS2_PLACEMENT_3D('',#10547,#8438,#8439);
#7620=AXIS2_PLACEMENT_3D('',#10549,#8440,#8441);
#7621=AXIS2_PLACEMENT_3D('',#10552,#8443,#8444);
#7622=AXIS2_PLACEMENT_3D('',#10553,#8445,#8446);
#7623=AXIS2_PLACEMENT_3D('',#10562,#8451,#8452);
#7624=AXIS2_PLACEMENT_3D('',#10568,#8456,#8457);
#7625=AXIS2_PLACEMENT_3D('',#10574,#8461,#8462);
#7626=AXIS2_PLACEMENT_3D('',#10580,#8466,#8467);
#7627=AXIS2_PLACEMENT_3D('',#10586,#8471,#8472);
#7628=AXIS2_PLACEMENT_3D('',#10592,#8476,#8477);
#7629=AXIS2_PLACEMENT_3D('',#10598,#8481,#8482);
#7630=AXIS2_PLACEMENT_3D('',#10604,#8486,#8487);
#7631=AXIS2_PLACEMENT_3D('',#10610,#8491,#8492);
#7632=AXIS2_PLACEMENT_3D('',#10616,#8496,#8497);
#7633=AXIS2_PLACEMENT_3D('',#10622,#8501,#8502);
#7634=AXIS2_PLACEMENT_3D('',#10628,#8506,#8507);
#7635=AXIS2_PLACEMENT_3D('',#10634,#8511,#8512);
#7636=AXIS2_PLACEMENT_3D('',#10640,#8516,#8517);
#7637=AXIS2_PLACEMENT_3D('',#10646,#8521,#8522);
#7638=AXIS2_PLACEMENT_3D('',#10652,#8526,#8527);
#7639=AXIS2_PLACEMENT_3D('',#10658,#8531,#8532);
#7640=AXIS2_PLACEMENT_3D('',#10661,#8535,#8536);
#7641=AXIS2_PLACEMENT_3D('',#10662,#8537,#8538);
#7642=AXIS2_PLACEMENT_3D('',#10663,#8539,#8540);
#7643=AXIS2_PLACEMENT_3D('',#10664,#8541,#8542);
#7644=AXIS2_PLACEMENT_3D('',#10665,#8543,#8544);
#7645=AXIS2_PLACEMENT_3D('',#10666,#8545,#8546);
#7646=AXIS2_PLACEMENT_3D('',#10667,#8547,#8548);
#7647=AXIS2_PLACEMENT_3D('',#10668,#8549,#8550);
#7648=AXIS2_PLACEMENT_3D('',#10669,#8551,#8552);
#7649=AXIS2_PLACEMENT_3D('',#10670,#8553,#8554);
#7650=AXIS2_PLACEMENT_3D('',#10671,#8555,#8556);
#7651=AXIS2_PLACEMENT_3D('',#10672,#8557,#8558);
#7652=AXIS2_PLACEMENT_3D('',#10673,#8559,#8560);
#7653=AXIS2_PLACEMENT_3D('',#10674,#8561,#8562);
#7654=AXIS2_PLACEMENT_3D('',#10675,#8563,#8564);
#7655=AXIS2_PLACEMENT_3D('',#10676,#8565,#8566);
#7656=AXIS2_PLACEMENT_3D('',#10677,#8567,#8568);
#7657=AXIS2_PLACEMENT_3D('',#10678,#8569,#8570);
#7658=AXIS2_PLACEMENT_3D('',#10680,#8571,#8572);
#7659=AXIS2_PLACEMENT_3D('',#10702,#8583,#8584);
#7660=AXIS2_PLACEMENT_3D('',#10724,#8595,#8596);
#7661=AXIS2_PLACEMENT_3D('',#10725,#8597,#8598);
#7662=AXIS2_PLACEMENT_3D('',#10726,#8599,#8600);
#7663=AXIS2_PLACEMENT_3D('',#10734,#8605,#8606);
#7664=AXIS2_PLACEMENT_3D('',#10740,#8610,#8611);
#7665=AXIS2_PLACEMENT_3D('',#10746,#8615,#8616);
#7666=AXIS2_PLACEMENT_3D('',#10752,#8620,#8621);
#7667=AXIS2_PLACEMENT_3D('',#10758,#8625,#8626);
#7668=AXIS2_PLACEMENT_3D('',#10764,#8630,#8631);
#7669=AXIS2_PLACEMENT_3D('',#10770,#8635,#8636);
#7670=AXIS2_PLACEMENT_3D('',#10775,#8640,#8641);
#7671=AXIS2_PLACEMENT_3D('',#10779,#8644,#8645);
#7672=AXIS2_PLACEMENT_3D('',#10783,#8648,#8649);
#7673=AXIS2_PLACEMENT_3D('',#10787,#8652,#8653);
#7674=AXIS2_PLACEMENT_3D('',#10791,#8656,#8657);
#7675=AXIS2_PLACEMENT_3D('',#10795,#8660,#8661);
#7676=AXIS2_PLACEMENT_3D('',#10799,#8664,#8665);
#7677=AXIS2_PLACEMENT_3D('',#10803,#8668,#8669);
#7678=AXIS2_PLACEMENT_3D('',#10807,#8672,#8673);
#7679=AXIS2_PLACEMENT_3D('',#10811,#8676,#8677);
#7680=AXIS2_PLACEMENT_3D('',#10813,#8679,#8680);
#7681=AXIS2_PLACEMENT_3D('',#10814,#8681,#8682);
#7682=AXIS2_PLACEMENT_3D('',#10815,#8683,#8684);
#7683=AXIS2_PLACEMENT_3D('',#10816,#8685,#8686);
#7684=AXIS2_PLACEMENT_3D('',#10817,#8687,#8688);
#7685=AXIS2_PLACEMENT_3D('',#10818,#8689,#8690);
#7686=AXIS2_PLACEMENT_3D('',#10819,#8691,#8692);
#7687=AXIS2_PLACEMENT_3D('',#10820,#8693,#8694);
#7688=AXIS2_PLACEMENT_3D('',#10821,#8695,#8696);
#7689=AXIS2_PLACEMENT_3D('',#10822,#8697,#8698);
#7690=AXIS2_PLACEMENT_3D('',#10823,#8699,#8700);
#7691=AXIS2_PLACEMENT_3D('',#10824,#8701,#8702);
#7692=AXIS2_PLACEMENT_3D('',#10825,#8703,#8704);
#7693=AXIS2_PLACEMENT_3D('',#10826,#8705,#8706);
#7694=AXIS2_PLACEMENT_3D('',#10827,#8707,#8708);
#7695=AXIS2_PLACEMENT_3D('',#10828,#8709,#8710);
#7696=AXIS2_PLACEMENT_3D('',#10829,#8711,#8712);
#7697=AXIS2_PLACEMENT_3D('',#10830,#8713,#8714);
#7698=AXIS2_PLACEMENT_3D('',#10838,#8719,#8720);
#7699=AXIS2_PLACEMENT_3D('',#10844,#8724,#8725);
#7700=AXIS2_PLACEMENT_3D('',#10850,#8729,#8730);
#7701=AXIS2_PLACEMENT_3D('',#10856,#8734,#8735);
#7702=AXIS2_PLACEMENT_3D('',#10862,#8739,#8740);
#7703=AXIS2_PLACEMENT_3D('',#10868,#8744,#8745);
#7704=AXIS2_PLACEMENT_3D('',#10874,#8749,#8750);
#7705=AXIS2_PLACEMENT_3D('',#10879,#8754,#8755);
#7706=AXIS2_PLACEMENT_3D('',#10883,#8758,#8759);
#7707=AXIS2_PLACEMENT_3D('',#10887,#8762,#8763);
#7708=AXIS2_PLACEMENT_3D('',#10891,#8766,#8767);
#7709=AXIS2_PLACEMENT_3D('',#10895,#8770,#8771);
#7710=AXIS2_PLACEMENT_3D('',#10899,#8774,#8775);
#7711=AXIS2_PLACEMENT_3D('',#10903,#8778,#8779);
#7712=AXIS2_PLACEMENT_3D('',#10907,#8782,#8783);
#7713=AXIS2_PLACEMENT_3D('',#10911,#8786,#8787);
#7714=AXIS2_PLACEMENT_3D('',#10915,#8790,#8791);
#7715=AXIS2_PLACEMENT_3D('',#10917,#8793,#8794);
#7716=AXIS2_PLACEMENT_3D('',#10918,#8795,#8796);
#7717=AXIS2_PLACEMENT_3D('',#10919,#8797,#8798);
#7718=AXIS2_PLACEMENT_3D('',#10920,#8799,#8800);
#7719=AXIS2_PLACEMENT_3D('',#10921,#8801,#8802);
#7720=AXIS2_PLACEMENT_3D('',#10922,#8803,#8804);
#7721=AXIS2_PLACEMENT_3D('',#10923,#8805,#8806);
#7722=AXIS2_PLACEMENT_3D('',#10924,#8807,#8808);
#7723=AXIS2_PLACEMENT_3D('',#10925,#8809,#8810);
#7724=AXIS2_PLACEMENT_3D('',#10926,#8811,#8812);
#7725=AXIS2_PLACEMENT_3D('',#10927,#8813,#8814);
#7726=AXIS2_PLACEMENT_3D('',#10928,#8815,#8816);
#7727=AXIS2_PLACEMENT_3D('',#10929,#8817,#8818);
#7728=AXIS2_PLACEMENT_3D('',#10930,#8819,#8820);
#7729=AXIS2_PLACEMENT_3D('',#10931,#8821,#8822);
#7730=AXIS2_PLACEMENT_3D('',#10932,#8823,#8824);
#7731=AXIS2_PLACEMENT_3D('',#10933,#8825,#8826);
#7732=AXIS2_PLACEMENT_3D('',#10934,#8827,#8828);
#7733=AXIS2_PLACEMENT_3D('',#10936,#8829,#8830);
#7734=AXIS2_PLACEMENT_3D('',#10938,#8832,#8833);
#7735=AXIS2_PLACEMENT_3D('',#10939,#8834,#8835);
#7736=AXIS2_PLACEMENT_3D('',#10940,#8836,#8837);
#7737=AXIS2_PLACEMENT_3D('',#11018,#8839,#8840);
#7738=AXIS2_PLACEMENT_3D('',#11020,#8841,#8842);
#7739=AXIS2_PLACEMENT_3D('',#11023,#8844,#8845);
#7740=AXIS2_PLACEMENT_3D('',#11024,#8846,#8847);
#7741=AXIS2_PLACEMENT_3D('',#11033,#8852,#8853);
#7742=AXIS2_PLACEMENT_3D('',#11039,#8857,#8858);
#7743=AXIS2_PLACEMENT_3D('',#11045,#8862,#8863);
#7744=AXIS2_PLACEMENT_3D('',#11051,#8867,#8868);
#7745=AXIS2_PLACEMENT_3D('',#11057,#8872,#8873);
#7746=AXIS2_PLACEMENT_3D('',#11063,#8877,#8878);
#7747=AXIS2_PLACEMENT_3D('',#11069,#8882,#8883);
#7748=AXIS2_PLACEMENT_3D('',#11075,#8887,#8888);
#7749=AXIS2_PLACEMENT_3D('',#11081,#8892,#8893);
#7750=AXIS2_PLACEMENT_3D('',#11087,#8897,#8898);
#7751=AXIS2_PLACEMENT_3D('',#11093,#8902,#8903);
#7752=AXIS2_PLACEMENT_3D('',#11099,#8907,#8908);
#7753=AXIS2_PLACEMENT_3D('',#11105,#8912,#8913);
#7754=AXIS2_PLACEMENT_3D('',#11111,#8917,#8918);
#7755=AXIS2_PLACEMENT_3D('',#11117,#8922,#8923);
#7756=AXIS2_PLACEMENT_3D('',#11123,#8927,#8928);
#7757=AXIS2_PLACEMENT_3D('',#11129,#8932,#8933);
#7758=AXIS2_PLACEMENT_3D('',#11132,#8936,#8937);
#7759=AXIS2_PLACEMENT_3D('',#11133,#8938,#8939);
#7760=AXIS2_PLACEMENT_3D('',#11134,#8940,#8941);
#7761=AXIS2_PLACEMENT_3D('',#11135,#8942,#8943);
#7762=AXIS2_PLACEMENT_3D('',#11136,#8944,#8945);
#7763=AXIS2_PLACEMENT_3D('',#11137,#8946,#8947);
#7764=AXIS2_PLACEMENT_3D('',#11138,#8948,#8949);
#7765=AXIS2_PLACEMENT_3D('',#11139,#8950,#8951);
#7766=AXIS2_PLACEMENT_3D('',#11140,#8952,#8953);
#7767=AXIS2_PLACEMENT_3D('',#11141,#8954,#8955);
#7768=AXIS2_PLACEMENT_3D('',#11142,#8956,#8957);
#7769=AXIS2_PLACEMENT_3D('',#11143,#8958,#8959);
#7770=AXIS2_PLACEMENT_3D('',#11144,#8960,#8961);
#7771=AXIS2_PLACEMENT_3D('',#11145,#8962,#8963);
#7772=AXIS2_PLACEMENT_3D('',#11147,#8964,#8965);
#7773=AXIS2_PLACEMENT_3D('',#11149,#8966,#8967);
#7774=AXIS2_PLACEMENT_3D('',#11171,#8978,#8979);
#7775=AXIS2_PLACEMENT_3D('',#11192,#8990,#8991);
#7776=AXIS2_PLACEMENT_3D('',#11193,#8992,#8993);
#7777=AXIS2_PLACEMENT_3D('',#11194,#8994,#8995);
#7778=AXIS2_PLACEMENT_3D('',#11195,#8996,#8997);
#7779=AXIS2_PLACEMENT_3D('',#11196,#8998,#8999);
#7780=AXIS2_PLACEMENT_3D('',#11197,#9000,#9001);
#7781=AXIS2_PLACEMENT_3D('',#11203,#9005,#9006);
#7782=AXIS2_PLACEMENT_3D('',#11207,#9009,#9010);
#7783=AXIS2_PLACEMENT_3D('',#11211,#9013,#9014);
#7784=AXIS2_PLACEMENT_3D('',#11215,#9017,#9018);
#7785=AXIS2_PLACEMENT_3D('',#11219,#9021,#9022);
#7786=AXIS2_PLACEMENT_3D('',#11223,#9025,#9026);
#7787=AXIS2_PLACEMENT_3D('',#11227,#9029,#9030);
#7788=AXIS2_PLACEMENT_3D('',#11231,#9033,#9034);
#7789=AXIS2_PLACEMENT_3D('',#11235,#9037,#9038);
#7790=AXIS2_PLACEMENT_3D('',#11241,#9042,#9043);
#7791=AXIS2_PLACEMENT_3D('',#11247,#9047,#9048);
#7792=AXIS2_PLACEMENT_3D('',#11253,#9052,#9053);
#7793=AXIS2_PLACEMENT_3D('',#11259,#9057,#9058);
#7794=AXIS2_PLACEMENT_3D('',#11265,#9062,#9063);
#7795=AXIS2_PLACEMENT_3D('',#11271,#9067,#9068);
#7796=AXIS2_PLACEMENT_3D('',#11277,#9072,#9073);
#7797=AXIS2_PLACEMENT_3D('',#11282,#9077,#9078);
#7798=AXIS2_PLACEMENT_3D('',#11284,#9080,#9081);
#7799=AXIS2_PLACEMENT_3D('',#11285,#9082,#9083);
#7800=AXIS2_PLACEMENT_3D('',#11286,#9084,#9085);
#7801=AXIS2_PLACEMENT_3D('',#11287,#9086,#9087);
#7802=AXIS2_PLACEMENT_3D('',#11288,#9088,#9089);
#7803=AXIS2_PLACEMENT_3D('',#11289,#9090,#9091);
#7804=AXIS2_PLACEMENT_3D('',#11290,#9092,#9093);
#7805=AXIS2_PLACEMENT_3D('',#11291,#9094,#9095);
#7806=AXIS2_PLACEMENT_3D('',#11292,#9096,#9097);
#7807=AXIS2_PLACEMENT_3D('',#11293,#9098,#9099);
#7808=AXIS2_PLACEMENT_3D('',#11294,#9100,#9101);
#7809=AXIS2_PLACEMENT_3D('',#11295,#9102,#9103);
#7810=AXIS2_PLACEMENT_3D('',#11296,#9104,#9105);
#7811=AXIS2_PLACEMENT_3D('',#11297,#9106,#9107);
#7812=AXIS2_PLACEMENT_3D('',#11298,#9108,#9109);
#7813=AXIS2_PLACEMENT_3D('',#11299,#9110,#9111);
#7814=AXIS2_PLACEMENT_3D('',#11300,#9112,#9113);
#7815=AXIS2_PLACEMENT_3D('',#11301,#9114,#9115);
#7816=AXIS2_PLACEMENT_3D('',#11307,#9119,#9120);
#7817=AXIS2_PLACEMENT_3D('',#11311,#9123,#9124);
#7818=AXIS2_PLACEMENT_3D('',#11315,#9127,#9128);
#7819=AXIS2_PLACEMENT_3D('',#11319,#9131,#9132);
#7820=AXIS2_PLACEMENT_3D('',#11323,#9135,#9136);
#7821=AXIS2_PLACEMENT_3D('',#11327,#9139,#9140);
#7822=AXIS2_PLACEMENT_3D('',#11331,#9143,#9144);
#7823=AXIS2_PLACEMENT_3D('',#11335,#9147,#9148);
#7824=AXIS2_PLACEMENT_3D('',#11339,#9151,#9152);
#7825=AXIS2_PLACEMENT_3D('',#11345,#9156,#9157);
#7826=AXIS2_PLACEMENT_3D('',#11351,#9161,#9162);
#7827=AXIS2_PLACEMENT_3D('',#11357,#9166,#9167);
#7828=AXIS2_PLACEMENT_3D('',#11363,#9171,#9172);
#7829=AXIS2_PLACEMENT_3D('',#11369,#9176,#9177);
#7830=AXIS2_PLACEMENT_3D('',#11375,#9181,#9182);
#7831=AXIS2_PLACEMENT_3D('',#11381,#9186,#9187);
#7832=AXIS2_PLACEMENT_3D('',#11386,#9191,#9192);
#7833=AXIS2_PLACEMENT_3D('',#11388,#9194,#9195);
#7834=AXIS2_PLACEMENT_3D('',#11389,#9196,#9197);
#7835=AXIS2_PLACEMENT_3D('',#11390,#9198,#9199);
#7836=AXIS2_PLACEMENT_3D('',#11391,#9200,#9201);
#7837=AXIS2_PLACEMENT_3D('',#11392,#9202,#9203);
#7838=AXIS2_PLACEMENT_3D('',#11393,#9204,#9205);
#7839=AXIS2_PLACEMENT_3D('',#11394,#9206,#9207);
#7840=AXIS2_PLACEMENT_3D('',#11395,#9208,#9209);
#7841=AXIS2_PLACEMENT_3D('',#11396,#9210,#9211);
#7842=AXIS2_PLACEMENT_3D('',#11397,#9212,#9213);
#7843=AXIS2_PLACEMENT_3D('',#11398,#9214,#9215);
#7844=AXIS2_PLACEMENT_3D('',#11399,#9216,#9217);
#7845=AXIS2_PLACEMENT_3D('',#11400,#9218,#9219);
#7846=AXIS2_PLACEMENT_3D('',#11401,#9220,#9221);
#7847=AXIS2_PLACEMENT_3D('',#11402,#9222,#9223);
#7848=AXIS2_PLACEMENT_3D('',#11403,#9224,#9225);
#7849=AXIS2_PLACEMENT_3D('',#11404,#9226,#9227);
#7850=AXIS2_PLACEMENT_3D('',#11405,#9228,#9229);
#7851=AXIS2_PLACEMENT_3D('',#11407,#9230,#9231);
#7852=AXIS2_PLACEMENT_3D('',#11409,#9233,#9234);
#7853=AXIS2_PLACEMENT_3D('',#11410,#9235,#9236);
#7854=AXIS2_PLACEMENT_3D('',#11411,#9237,#9238);
#7855=AXIS2_PLACEMENT_3D('',#11430,#9247,#9248);
#7856=AXIS2_PLACEMENT_3D('',#11448,#9257,#9258);
#7857=AXIS2_PLACEMENT_3D('',#11466,#9267,#9268);
#7858=AXIS2_PLACEMENT_3D('',#11484,#9277,#9278);
#7859=AXIS2_PLACEMENT_3D('',#11502,#9287,#9288);
#7860=AXIS2_PLACEMENT_3D('',#11519,#9297,#9298);
#7861=AXIS2_PLACEMENT_3D('',#11520,#9299,#9300);
#7862=AXIS2_PLACEMENT_3D('',#11524,#9302,#9303);
#7863=AXIS2_PLACEMENT_3D('',#11526,#9305,#9306);
#7864=AXIS2_PLACEMENT_3D('',#11530,#9308,#9309);
#7865=AXIS2_PLACEMENT_3D('',#11532,#9311,#9312);
#7866=AXIS2_PLACEMENT_3D('',#11536,#9314,#9315);
#7867=AXIS2_PLACEMENT_3D('',#11538,#9317,#9318);
#7868=AXIS2_PLACEMENT_3D('',#11543,#9321,#9322);
#7869=AXIS2_PLACEMENT_3D('',#11544,#9323,#9324);
#7870=AXIS2_PLACEMENT_3D('',#11549,#9327,#9328);
#7871=AXIS2_PLACEMENT_3D('',#11550,#9329,#9330);
#7872=AXIS2_PLACEMENT_3D('',#11555,#9333,#9334);
#7873=AXIS2_PLACEMENT_3D('',#11556,#9335,#9336);
#7874=AXIS2_PLACEMENT_3D('',#11647,#9385,#9386);
#7875=AXIS2_PLACEMENT_3D('',#11657,#9392,#9393);
#7876=AXIS2_PLACEMENT_3D('',#11661,#9396,#9397);
#7877=AXIS2_PLACEMENT_3D('',#11665,#9400,#9401);
#7878=AXIS2_PLACEMENT_3D('',#11669,#9404,#9405);
#7879=AXIS2_PLACEMENT_3D('',#11673,#9408,#9409);
#7880=AXIS2_PLACEMENT_3D('',#11677,#9412,#9413);
#7881=AXIS2_PLACEMENT_3D('',#11681,#9416,#9417);
#7882=AXIS2_PLACEMENT_3D('',#11685,#9420,#9421);
#7883=AXIS2_PLACEMENT_3D('',#11709,#9434,#9435);
#7884=AXIS2_PLACEMENT_3D('',#11712,#9438,#9439);
#7885=AXIS2_PLACEMENT_3D('',#11714,#9441,#9442);
#7886=AXIS2_PLACEMENT_3D('',#11716,#9444,#9445);
#7887=AXIS2_PLACEMENT_3D('',#11718,#9447,#9448);
#7888=AXIS2_PLACEMENT_3D('',#11719,#9449,#9450);
#7889=AXIS2_PLACEMENT_3D('',#11723,#9453,#9454);
#7890=AXIS2_PLACEMENT_3D('',#11727,#9457,#9458);
#7891=AXIS2_PLACEMENT_3D('',#11731,#9461,#9462);
#7892=AXIS2_PLACEMENT_3D('',#11735,#9465,#9466);
#7893=AXIS2_PLACEMENT_3D('',#11739,#9469,#9470);
#7894=AXIS2_PLACEMENT_3D('',#11743,#9473,#9474);
#7895=AXIS2_PLACEMENT_3D('',#11745,#9476,#9477);
#7896=AXIS2_PLACEMENT_3D('',#11746,#9478,#9479);
#7897=AXIS2_PLACEMENT_3D('',#11756,#9485,#9486);
#7898=AXIS2_PLACEMENT_3D('',#11760,#9489,#9490);
#7899=AXIS2_PLACEMENT_3D('',#11764,#9493,#9494);
#7900=AXIS2_PLACEMENT_3D('',#11768,#9497,#9498);
#7901=AXIS2_PLACEMENT_3D('',#11772,#9501,#9502);
#7902=AXIS2_PLACEMENT_3D('',#11776,#9505,#9506);
#7903=AXIS2_PLACEMENT_3D('',#11780,#9509,#9510);
#7904=AXIS2_PLACEMENT_3D('',#11784,#9513,#9514);
#7905=AXIS2_PLACEMENT_3D('',#11808,#9527,#9528);
#7906=AXIS2_PLACEMENT_3D('',#11811,#9531,#9532);
#7907=AXIS2_PLACEMENT_3D('',#11813,#9534,#9535);
#7908=AXIS2_PLACEMENT_3D('',#11815,#9537,#9538);
#7909=AXIS2_PLACEMENT_3D('',#11817,#9540,#9541);
#7910=AXIS2_PLACEMENT_3D('',#11818,#9542,#9543);
#7911=AXIS2_PLACEMENT_3D('',#11822,#9546,#9547);
#7912=AXIS2_PLACEMENT_3D('',#11826,#9550,#9551);
#7913=AXIS2_PLACEMENT_3D('',#11830,#9554,#9555);
#7914=AXIS2_PLACEMENT_3D('',#11834,#9558,#9559);
#7915=AXIS2_PLACEMENT_3D('',#11838,#9562,#9563);
#7916=AXIS2_PLACEMENT_3D('',#11842,#9566,#9567);
#7917=AXIS2_PLACEMENT_3D('',#11844,#9569,#9570);
#7918=AXIS2_PLACEMENT_3D('',#11845,#9571,#9572);
#7919=AXIS2_PLACEMENT_3D('',#11855,#9578,#9579);
#7920=AXIS2_PLACEMENT_3D('',#11859,#9582,#9583);
#7921=AXIS2_PLACEMENT_3D('',#11863,#9586,#9587);
#7922=AXIS2_PLACEMENT_3D('',#11867,#9590,#9591);
#7923=AXIS2_PLACEMENT_3D('',#11871,#9594,#9595);
#7924=AXIS2_PLACEMENT_3D('',#11875,#9598,#9599);
#7925=AXIS2_PLACEMENT_3D('',#11879,#9602,#9603);
#7926=AXIS2_PLACEMENT_3D('',#11883,#9606,#9607);
#7927=AXIS2_PLACEMENT_3D('',#11907,#9620,#9621);
#7928=AXIS2_PLACEMENT_3D('',#11910,#9624,#9625);
#7929=AXIS2_PLACEMENT_3D('',#11912,#9627,#9628);
#7930=AXIS2_PLACEMENT_3D('',#11914,#9630,#9631);
#7931=AXIS2_PLACEMENT_3D('',#11916,#9633,#9634);
#7932=AXIS2_PLACEMENT_3D('',#11917,#9635,#9636);
#7933=AXIS2_PLACEMENT_3D('',#11921,#9639,#9640);
#7934=AXIS2_PLACEMENT_3D('',#11925,#9643,#9644);
#7935=AXIS2_PLACEMENT_3D('',#11929,#9647,#9648);
#7936=AXIS2_PLACEMENT_3D('',#11933,#9651,#9652);
#7937=AXIS2_PLACEMENT_3D('',#11937,#9655,#9656);
#7938=AXIS2_PLACEMENT_3D('',#11941,#9659,#9660);
#7939=AXIS2_PLACEMENT_3D('',#11943,#9662,#9663);
#7940=AXIS2_PLACEMENT_3D('',#11944,#9664,#9665);
#7941=AXIS2_PLACEMENT_3D('',#11954,#9671,#9672);
#7942=AXIS2_PLACEMENT_3D('',#11958,#9675,#9676);
#7943=AXIS2_PLACEMENT_3D('',#11962,#9679,#9680);
#7944=AXIS2_PLACEMENT_3D('',#11966,#9683,#9684);
#7945=AXIS2_PLACEMENT_3D('',#11970,#9687,#9688);
#7946=AXIS2_PLACEMENT_3D('',#11974,#9691,#9692);
#7947=AXIS2_PLACEMENT_3D('',#11978,#9695,#9696);
#7948=AXIS2_PLACEMENT_3D('',#11982,#9699,#9700);
#7949=AXIS2_PLACEMENT_3D('',#12006,#9713,#9714);
#7950=AXIS2_PLACEMENT_3D('',#12009,#9717,#9718);
#7951=AXIS2_PLACEMENT_3D('',#12011,#9720,#9721);
#7952=AXIS2_PLACEMENT_3D('',#12013,#9723,#9724);
#7953=AXIS2_PLACEMENT_3D('',#12015,#9726,#9727);
#7954=AXIS2_PLACEMENT_3D('',#12016,#9728,#9729);
#7955=AXIS2_PLACEMENT_3D('',#12020,#9732,#9733);
#7956=AXIS2_PLACEMENT_3D('',#12024,#9736,#9737);
#7957=AXIS2_PLACEMENT_3D('',#12028,#9740,#9741);
#7958=AXIS2_PLACEMENT_3D('',#12032,#9744,#9745);
#7959=AXIS2_PLACEMENT_3D('',#12036,#9748,#9749);
#7960=AXIS2_PLACEMENT_3D('',#12040,#9752,#9753);
#7961=AXIS2_PLACEMENT_3D('',#12042,#9755,#9756);
#7962=AXIS2_PLACEMENT_3D('',#12043,#9757,#9758);
#7963=AXIS2_PLACEMENT_3D('',#12053,#9764,#9765);
#7964=AXIS2_PLACEMENT_3D('',#12057,#9768,#9769);
#7965=AXIS2_PLACEMENT_3D('',#12061,#9772,#9773);
#7966=AXIS2_PLACEMENT_3D('',#12065,#9776,#9777);
#7967=AXIS2_PLACEMENT_3D('',#12069,#9780,#9781);
#7968=AXIS2_PLACEMENT_3D('',#12073,#9784,#9785);
#7969=AXIS2_PLACEMENT_3D('',#12077,#9788,#9789);
#7970=AXIS2_PLACEMENT_3D('',#12081,#9792,#9793);
#7971=AXIS2_PLACEMENT_3D('',#12105,#9806,#9807);
#7972=AXIS2_PLACEMENT_3D('',#12108,#9810,#9811);
#7973=AXIS2_PLACEMENT_3D('',#12110,#9813,#9814);
#7974=AXIS2_PLACEMENT_3D('',#12112,#9816,#9817);
#7975=AXIS2_PLACEMENT_3D('',#12114,#9819,#9820);
#7976=AXIS2_PLACEMENT_3D('',#12115,#9821,#9822);
#7977=AXIS2_PLACEMENT_3D('',#12119,#9825,#9826);
#7978=AXIS2_PLACEMENT_3D('',#12123,#9829,#9830);
#7979=AXIS2_PLACEMENT_3D('',#12127,#9833,#9834);
#7980=AXIS2_PLACEMENT_3D('',#12131,#9837,#9838);
#7981=AXIS2_PLACEMENT_3D('',#12135,#9841,#9842);
#7982=AXIS2_PLACEMENT_3D('',#12139,#9845,#9846);
#7983=AXIS2_PLACEMENT_3D('',#12141,#9848,#9849);
#7984=AXIS2_PLACEMENT_3D('',#12142,#9850,#9851);
#7985=AXIS2_PLACEMENT_3D('',#12152,#9857,#9858);
#7986=AXIS2_PLACEMENT_3D('',#12156,#9861,#9862);
#7987=AXIS2_PLACEMENT_3D('',#12160,#9865,#9866);
#7988=AXIS2_PLACEMENT_3D('',#12164,#9869,#9870);
#7989=AXIS2_PLACEMENT_3D('',#12168,#9873,#9874);
#7990=AXIS2_PLACEMENT_3D('',#12172,#9877,#9878);
#7991=AXIS2_PLACEMENT_3D('',#12176,#9881,#9882);
#7992=AXIS2_PLACEMENT_3D('',#12180,#9885,#9886);
#7993=AXIS2_PLACEMENT_3D('',#12204,#9899,#9900);
#7994=AXIS2_PLACEMENT_3D('',#12207,#9903,#9904);
#7995=AXIS2_PLACEMENT_3D('',#12209,#9906,#9907);
#7996=AXIS2_PLACEMENT_3D('',#12211,#9909,#9910);
#7997=AXIS2_PLACEMENT_3D('',#12213,#9912,#9913);
#7998=AXIS2_PLACEMENT_3D('',#12214,#9914,#9915);
#7999=AXIS2_PLACEMENT_3D('',#12218,#9918,#9919);
#8000=AXIS2_PLACEMENT_3D('',#12222,#9922,#9923);
#8001=AXIS2_PLACEMENT_3D('',#12226,#9926,#9927);
#8002=AXIS2_PLACEMENT_3D('',#12230,#9930,#9931);
#8003=AXIS2_PLACEMENT_3D('',#12234,#9934,#9935);
#8004=AXIS2_PLACEMENT_3D('',#12238,#9938,#9939);
#8005=AXIS2_PLACEMENT_3D('',#12240,#9941,#9942);
#8006=AXIS2_PLACEMENT_3D('',#12241,#9943,#9944);
#8007=AXIS2_PLACEMENT_3D('',#12242,#9945,#9946);
#8008=AXIS2_PLACEMENT_3D('',#12243,#9947,#9948);
#8009=AXIS2_PLACEMENT_3D('',#12244,#9949,#9950);
#8010=AXIS2_PLACEMENT_3D('',#12245,#9951,#9952);
#8011=AXIS2_PLACEMENT_3D('',#12254,#9957,#9958);
#8012=AXIS2_PLACEMENT_3D('',#12260,#9962,#9963);
#8013=AXIS2_PLACEMENT_3D('',#12266,#9967,#9968);
#8014=AXIS2_PLACEMENT_3D('',#12272,#9972,#9973);
#8015=AXIS2_PLACEMENT_3D('',#12278,#9977,#9978);
#8016=AXIS2_PLACEMENT_3D('',#12281,#9981,#9982);
#8017=AXIS2_PLACEMENT_3D('',#12282,#9983,#9984);
#8018=AXIS2_PLACEMENT_3D('',#12284,#9985,#9986);
#8019=AXIS2_PLACEMENT_3D('',#12285,#9987,#9988);
#8020=AXIS2_PLACEMENT_3D('',#12287,#9989,#9990);
#8021=AXIS2_PLACEMENT_3D('',#12289,#9992,#9993);
#8022=AXIS2_PLACEMENT_3D('',#12291,#9994,#9995);
#8023=AXIS2_PLACEMENT_3D('',#12293,#9997,#9998);
#8024=AXIS2_PLACEMENT_3D('',#12295,#9999,#10000);
#8025=AXIS2_PLACEMENT_3D('',#12297,#10002,#10003);
#8026=AXIS2_PLACEMENT_3D('',#12298,#10004,#10005);
#8027=AXIS2_PLACEMENT_3D('',#12299,#10006,#10007);
#8028=AXIS2_PLACEMENT_3D('',#12300,#10008,#10009);
#8029=AXIS2_PLACEMENT_3D('',#12301,#10010,#10011);
#8030=AXIS2_PLACEMENT_3D('',#12302,#10012,#10013);
#8031=AXIS2_PLACEMENT_3D('',#12303,#10014,#10015);
#8032=AXIS2_PLACEMENT_3D('',#12304,#10016,#10017);
#8033=AXIS2_PLACEMENT_3D('',#12305,#10018,#10019);
#8034=AXIS2_PLACEMENT_3D('',#12306,#10020,#10021);
#8035=AXIS2_PLACEMENT_3D('',#12307,#10022,#10023);
#8036=AXIS2_PLACEMENT_3D('',#12308,#10024,#10025);
#8037=AXIS2_PLACEMENT_3D('',#12309,#10026,#10027);
#8038=AXIS2_PLACEMENT_3D('',#12310,#10028,#10029);
#8039=AXIS2_PLACEMENT_3D('',#12311,#10030,#10031);
#8040=AXIS2_PLACEMENT_3D('',#12312,#10032,#10033);
#8041=AXIS2_PLACEMENT_3D('',#12313,#10034,#10035);
#8042=AXIS2_PLACEMENT_3D('',#12314,#10036,#10037);
#8043=AXIS2_PLACEMENT_3D('',#12315,#10038,#10039);
#8044=DIRECTION('axis',(0.,0.,1.));
#8045=DIRECTION('refdir',(1.,0.,0.));
#8046=DIRECTION('axis',(0.,0.,1.));
#8047=DIRECTION('refdir',(1.,0.,0.));
#8048=DIRECTION('center_axis',(0.,0.,1.));
#8049=DIRECTION('ref_axis',(1.,0.,0.));
#8050=DIRECTION('center_axis',(0.,0.,1.));
#8051=DIRECTION('ref_axis',(1.,0.,0.));
#8052=DIRECTION('',(0.,0.,1.));
#8053=DIRECTION('center_axis',(0.,0.,-1.));
#8054=DIRECTION('ref_axis',(1.,0.,0.));
#8055=DIRECTION('center_axis',(0.,0.,1.));
#8056=DIRECTION('ref_axis',(1.,0.,0.));
#8057=DIRECTION('center_axis',(0.,0.,1.));
#8058=DIRECTION('ref_axis',(1.,0.,0.));
#8059=DIRECTION('',(0.,0.,1.));
#8060=DIRECTION('center_axis',(0.,0.,-1.));
#8061=DIRECTION('ref_axis',(1.,0.,0.));
#8062=DIRECTION('center_axis',(0.,0.,1.));
#8063=DIRECTION('ref_axis',(1.,0.,0.));
#8064=DIRECTION('center_axis',(0.,0.,1.));
#8065=DIRECTION('ref_axis',(1.,0.,0.));
#8066=DIRECTION('',(0.,0.,1.));
#8067=DIRECTION('center_axis',(0.,0.,-1.));
#8068=DIRECTION('ref_axis',(1.,0.,0.));
#8069=DIRECTION('center_axis',(0.,0.,1.));
#8070=DIRECTION('ref_axis',(1.,0.,0.));
#8071=DIRECTION('center_axis',(0.,0.,1.));
#8072=DIRECTION('ref_axis',(1.,0.,0.));
#8073=DIRECTION('',(0.,0.,1.));
#8074=DIRECTION('center_axis',(0.,0.,-1.));
#8075=DIRECTION('ref_axis',(1.,0.,0.));
#8076=DIRECTION('center_axis',(0.,1.,0.));
#8077=DIRECTION('ref_axis',(-1.,0.,0.));
#8078=DIRECTION('',(-1.,0.,0.));
#8079=DIRECTION('',(0.,0.,1.));
#8080=DIRECTION('',(-1.,0.,0.));
#8081=DIRECTION('',(0.,0.,1.));
#8082=DIRECTION('center_axis',(1.,0.,0.));
#8083=DIRECTION('ref_axis',(0.,1.,0.));
#8084=DIRECTION('',(0.,1.,0.));
#8085=DIRECTION('',(0.,1.,0.));
#8086=DIRECTION('',(0.,0.,1.));
#8087=DIRECTION('center_axis',(0.,-1.,0.));
#8088=DIRECTION('ref_axis',(1.,0.,0.));
#8089=DIRECTION('',(1.,0.,0.));
#8090=DIRECTION('',(1.,0.,0.));
#8091=DIRECTION('',(0.,0.,1.));
#8092=DIRECTION('center_axis',(-1.,0.,0.));
#8093=DIRECTION('ref_axis',(0.,-1.,0.));
#8094=DIRECTION('',(0.,-1.,0.));
#8095=DIRECTION('',(0.,-1.,0.));
#8096=DIRECTION('center_axis',(0.,0.,1.));
#8097=DIRECTION('ref_axis',(1.,0.,0.));
#8098=DIRECTION('center_axis',(0.,0.,1.));
#8099=DIRECTION('ref_axis',(1.,0.,0.));
#8100=DIRECTION('axis',(0.,0.,1.));
#8101=DIRECTION('refdir',(1.,0.,0.));
#8102=DIRECTION('center_axis',(0.,1.,0.));
#8103=DIRECTION('ref_axis',(1.,0.,0.));
#8104=DIRECTION('center_axis',(0.,1.,0.));
#8105=DIRECTION('ref_axis',(1.,0.,0.));
#8106=DIRECTION('',(0.,-1.,0.));
#8107=DIRECTION('center_axis',(0.,1.,0.));
#8108=DIRECTION('ref_axis',(1.,0.,0.));
#8109=DIRECTION('center_axis',(0.,1.,0.));
#8110=DIRECTION('ref_axis',(1.,0.,0.));
#8111=DIRECTION('center_axis',(0.,1.,0.));
#8112=DIRECTION('ref_axis',(1.,0.,0.));
#8113=DIRECTION('axis',(0.,0.,1.));
#8114=DIRECTION('refdir',(1.,0.,0.));
#8115=DIRECTION('center_axis',(0.,1.,0.));
#8116=DIRECTION('ref_axis',(1.,0.,0.));
#8117=DIRECTION('center_axis',(0.,1.,0.));
#8118=DIRECTION('ref_axis',(1.,0.,0.));
#8119=DIRECTION('',(0.,-1.,0.));
#8120=DIRECTION('center_axis',(0.,1.,0.));
#8121=DIRECTION('ref_axis',(1.,0.,0.));
#8122=DIRECTION('center_axis',(0.,1.,0.));
#8123=DIRECTION('ref_axis',(1.,0.,0.));
#8124=DIRECTION('center_axis',(0.,1.,0.));
#8125=DIRECTION('ref_axis',(1.,0.,0.));
#8126=DIRECTION('axis',(0.,0.,1.));
#8127=DIRECTION('refdir',(1.,0.,0.));
#8128=DIRECTION('center_axis',(0.,0.,1.));
#8129=DIRECTION('ref_axis',(1.,0.,0.));
#8130=DIRECTION('',(0.,-1.,0.));
#8131=DIRECTION('center_axis',(0.,0.,1.));
#8132=DIRECTION('ref_axis',(1.,0.,0.));
#8133=DIRECTION('center_axis',(0.,0.,1.));
#8134=DIRECTION('ref_axis',(1.,0.,0.));
#8135=DIRECTION('',(0.,0.,1.));
#8136=DIRECTION('center_axis',(0.,0.,1.));
#8137=DIRECTION('ref_axis',(1.,0.,0.));
#8138=DIRECTION('',(0.,0.,-1.));
#8139=DIRECTION('center_axis',(0.,0.,1.));
#8140=DIRECTION('ref_axis',(-1.,1.22464679914735E-16,0.));
#8141=DIRECTION('',(0.,0.,-1.));
#8142=DIRECTION('center_axis',(0.,0.,1.));
#8143=DIRECTION('ref_axis',(1.,0.,0.));
#8144=DIRECTION('',(0.,0.,1.));
#8145=DIRECTION('center_axis',(0.,0.,1.));
#8146=DIRECTION('ref_axis',(1.,0.,0.));
#8147=DIRECTION('center_axis',(0.,0.,1.));
#8148=DIRECTION('ref_axis',(1.,0.,0.));
#8149=DIRECTION('',(0.,1.,0.));
#8150=DIRECTION('center_axis',(0.,0.,1.));
#8151=DIRECTION('ref_axis',(1.,0.,0.));
#8152=DIRECTION('',(0.,1.,0.));
#8153=DIRECTION('',(1.,0.,0.));
#8154=DIRECTION('',(0.,-1.,0.));
#8155=DIRECTION('',(-1.,0.,0.));
#8156=DIRECTION('',(0.,1.,0.));
#8157=DIRECTION('center_axis',(0.,0.,-1.));
#8158=DIRECTION('ref_axis',(1.,0.,0.));
#8159=DIRECTION('center_axis',(-1.,0.,0.));
#8160=DIRECTION('ref_axis',(0.,0.,1.));
#8161=DIRECTION('',(0.,0.,-1.));
#8162=DIRECTION('',(0.,1.,0.));
#8163=DIRECTION('',(0.,0.,1.));
#8164=DIRECTION('center_axis',(1.,0.,0.));
#8165=DIRECTION('ref_axis',(0.,0.,-1.));
#8166=DIRECTION('center_axis',(0.,0.,1.));
#8167=DIRECTION('ref_axis',(1.,0.,0.));
#8168=DIRECTION('',(0.,1.,0.));
#8169=DIRECTION('',(1.,0.,0.));
#8170=DIRECTION('',(0.,1.,0.));
#8171=DIRECTION('',(0.,1.,0.));
#8172=DIRECTION('',(-1.,0.,0.));
#8173=DIRECTION('center_axis',(0.,0.,-1.));
#8174=DIRECTION('ref_axis',(1.,0.,0.));
#8175=DIRECTION('center_axis',(1.,0.,0.));
#8176=DIRECTION('ref_axis',(0.,0.,-1.));
#8177=DIRECTION('center_axis',(1.,0.,0.));
#8178=DIRECTION('ref_axis',(0.,0.,-1.));
#8179=DIRECTION('',(1.,0.,0.));
#8180=DIRECTION('center_axis',(-1.,0.,0.));
#8181=DIRECTION('ref_axis',(0.,0.,-1.));
#8182=DIRECTION('center_axis',(1.,0.,0.));
#8183=DIRECTION('ref_axis',(0.,0.,-1.));
#8184=DIRECTION('',(1.,0.,0.));
#8185=DIRECTION('center_axis',(-1.,0.,0.));
#8186=DIRECTION('ref_axis',(0.,0.,-1.));
#8187=DIRECTION('center_axis',(0.,0.,1.));
#8188=DIRECTION('ref_axis',(1.,0.,0.));
#8189=DIRECTION('center_axis',(0.,0.,1.));
#8190=DIRECTION('ref_axis',(1.,0.,0.));
#8191=DIRECTION('',(0.,0.,1.));
#8192=DIRECTION('center_axis',(0.,0.,1.));
#8193=DIRECTION('ref_axis',(1.,0.,0.));
#8194=DIRECTION('center_axis',(0.,0.,1.));
#8195=DIRECTION('ref_axis',(1.,0.,0.));
#8196=DIRECTION('',(0.,0.,1.));
#8197=DIRECTION('center_axis',(0.,1.,0.));
#8198=DIRECTION('ref_axis',(1.,0.,0.));
#8199=DIRECTION('center_axis',(0.,1.,0.));
#8200=DIRECTION('ref_axis',(1.,0.,0.));
#8201=DIRECTION('',(0.,1.,0.));
#8202=DIRECTION('center_axis',(0.,-1.,0.));
#8203=DIRECTION('ref_axis',(1.,0.,0.));
#8204=DIRECTION('center_axis',(0.,-1.,0.));
#8205=DIRECTION('ref_axis',(0.,0.,-1.));
#8206=DIRECTION('',(0.,0.,-1.));
#8207=DIRECTION('',(1.,0.,0.));
#8208=DIRECTION('',(0.,0.,1.));
#8209=DIRECTION('',(0.,0.,1.));
#8210=DIRECTION('',(-1.,0.,0.));
#8211=DIRECTION('',(0.,0.,-1.));
#8212=DIRECTION('',(-1.,0.,0.));
#8213=DIRECTION('',(0.,0.,1.));
#8214=DIRECTION('',(-1.,0.,0.));
#8215=DIRECTION('center_axis',(-1.,0.,0.));
#8216=DIRECTION('ref_axis',(0.,0.,1.));
#8217=DIRECTION('',(0.,0.,1.));
#8218=DIRECTION('',(0.,1.,0.));
#8219=DIRECTION('center_axis',(0.,0.,-1.));
#8220=DIRECTION('ref_axis',(-1.,0.,0.));
#8221=DIRECTION('',(-1.,0.,0.));
#8222=DIRECTION('',(0.,1.,0.));
#8223=DIRECTION('center_axis',(1.,0.,0.));
#8224=DIRECTION('ref_axis',(0.,0.,-1.));
#8225=DIRECTION('',(0.,0.,-1.));
#8226=DIRECTION('center_axis',(1.,0.,0.));
#8227=DIRECTION('ref_axis',(0.,0.,-1.));
#8228=DIRECTION('',(0.,0.,-1.));
#8229=DIRECTION('',(0.,1.,0.));
#8230=DIRECTION('center_axis',(0.,0.,1.));
#8231=DIRECTION('ref_axis',(1.,0.,0.));
#8232=DIRECTION('',(1.,0.,0.));
#8233=DIRECTION('',(0.,1.,0.));
#8234=DIRECTION('center_axis',(-1.,0.,0.));
#8235=DIRECTION('ref_axis',(0.,0.,1.));
#8236=DIRECTION('',(0.,0.,1.));
#8237=DIRECTION('',(0.,1.,0.));
#8238=DIRECTION('center_axis',(0.,0.,1.));
#8239=DIRECTION('ref_axis',(1.,0.,0.));
#8240=DIRECTION('',(1.,0.,0.));
#8241=DIRECTION('',(0.,1.,0.));
#8242=DIRECTION('center_axis',(1.,0.,0.));
#8243=DIRECTION('ref_axis',(0.,0.,-1.));
#8244=DIRECTION('',(0.,0.,-1.));
#8245=DIRECTION('',(0.,1.,0.));
#8246=DIRECTION('center_axis',(0.,0.,1.));
#8247=DIRECTION('ref_axis',(1.,0.,0.));
#8248=DIRECTION('',(1.,0.,0.));
#8249=DIRECTION('center_axis',(0.,1.,0.));
#8250=DIRECTION('ref_axis',(0.,0.,1.));
#8251=DIRECTION('axis',(0.,0.,1.));
#8252=DIRECTION('refdir',(1.,0.,0.));
#8253=DIRECTION('center_axis',(0.866025403784439,0.,-0.5));
#8254=DIRECTION('ref_axis',(0.5,0.,0.866025403784439));
#8255=DIRECTION('',(-0.5,0.,-0.866025403784439));
#8256=DIRECTION('',(0.,-1.,0.));
#8257=DIRECTION('',(0.5,0.,0.866025403784439));
#8258=DIRECTION('',(0.,-1.,0.));
#8259=DIRECTION('center_axis',(1.20185167898973E-16,0.,-1.));
#8260=DIRECTION('ref_axis',(1.,0.,1.20185167898973E-16));
#8261=DIRECTION('',(-1.,0.,-1.20185167898973E-16));
#8262=DIRECTION('',(0.,-1.,0.));
#8263=DIRECTION('',(1.,0.,1.20185167898973E-16));
#8264=DIRECTION('center_axis',(-0.866025403784439,0.,-0.5));
#8265=DIRECTION('ref_axis',(0.5,0.,-0.866025403784439));
#8266=DIRECTION('',(-0.5,0.,0.866025403784439));
#8267=DIRECTION('',(0.,-1.,0.));
#8268=DIRECTION('',(0.5,0.,-0.866025403784439));
#8269=DIRECTION('center_axis',(-0.866025403784439,0.,0.5));
#8270=DIRECTION('ref_axis',(-0.5,0.,-0.866025403784439));
#8271=DIRECTION('',(0.5,0.,0.866025403784439));
#8272=DIRECTION('',(0.,-1.,0.));
#8273=DIRECTION('',(-0.5,0.,-0.866025403784439));
#8274=DIRECTION('center_axis',(-2.40370335797945E-16,0.,1.));
#8275=DIRECTION('ref_axis',(-1.,0.,-2.40370335797945E-16));
#8276=DIRECTION('',(1.,0.,2.40370335797945E-16));
#8277=DIRECTION('',(0.,-1.,0.));
#8278=DIRECTION('',(-1.,0.,-2.40370335797945E-16));
#8279=DIRECTION('center_axis',(0.866025403784439,0.,0.5));
#8280=DIRECTION('ref_axis',(-0.5,0.,0.866025403784439));
#8281=DIRECTION('',(0.5,0.,-0.866025403784439));
#8282=DIRECTION('',(-0.5,0.,0.866025403784439));
#8283=DIRECTION('center_axis',(0.,1.,0.));
#8284=DIRECTION('ref_axis',(1.,0.,0.));
#8285=DIRECTION('center_axis',(0.,-1.,0.));
#8286=DIRECTION('ref_axis',(0.,0.,-1.));
#8287=DIRECTION('center_axis',(0.,1.,0.));
#8288=DIRECTION('ref_axis',(1.,0.,0.));
#8289=DIRECTION('center_axis',(0.,1.,0.));
#8290=DIRECTION('ref_axis',(1.,0.,0.));
#8291=DIRECTION('center_axis',(0.,1.,0.));
#8292=DIRECTION('ref_axis',(0.,0.,1.));
#8293=DIRECTION('center_axis',(0.,-1.,0.));
#8294=DIRECTION('ref_axis',(1.,0.,0.));
#8295=DIRECTION('center_axis',(0.,-1.,0.));
#8296=DIRECTION('ref_axis',(1.,0.,0.));
#8297=DIRECTION('center_axis',(0.,-1.,0.));
#8298=DIRECTION('ref_axis',(1.,0.,0.));
#8299=DIRECTION('',(0.707106781186548,0.707106781186547,8.65956056235493E-17));
#8300=DIRECTION('center_axis',(0.,-1.,0.));
#8301=DIRECTION('ref_axis',(1.,0.,0.));
#8302=DIRECTION('center_axis',(0.,-1.,0.));
#8303=DIRECTION('ref_axis',(1.,0.,0.));
#8304=DIRECTION('',(0.,1.,0.));
#8305=DIRECTION('center_axis',(0.,1.,0.));
#8306=DIRECTION('ref_axis',(1.,0.,0.));
#8307=DIRECTION('center_axis',(0.,-1.,0.));
#8308=DIRECTION('ref_axis',(1.,0.,0.));
#8309=DIRECTION('',(-0.707106781186547,0.707106781186548,-8.65956056235493E-17));
#8310=DIRECTION('center_axis',(0.,-1.,0.));
#8311=DIRECTION('ref_axis',(0.,0.,-1.));
#8312=DIRECTION('center_axis',(0.,-1.,0.));
#8313=DIRECTION('ref_axis',(1.,0.,0.));
#8314=DIRECTION('center_axis',(0.,1.,0.));
#8315=DIRECTION('ref_axis',(1.,0.,0.));
#8316=DIRECTION('center_axis',(0.,1.,0.));
#8317=DIRECTION('ref_axis',(1.,0.,0.));
#8318=DIRECTION('',(-0.447213595499958,0.894427190999916,-5.47678698264203E-17));
#8319=DIRECTION('center_axis',(0.,-1.,0.));
#8320=DIRECTION('ref_axis',(1.,0.,0.));
#8321=DIRECTION('',(0.,1.,0.));
#8322=DIRECTION('axis',(0.,0.,1.));
#8323=DIRECTION('refdir',(1.,0.,0.));
#8324=DIRECTION('center_axis',(0.,1.,0.));
#8325=DIRECTION('ref_axis',(0.,0.,1.));
#8326=DIRECTION('center_axis',(0.,-1.,0.));
#8327=DIRECTION('ref_axis',(1.,0.,0.));
#8328=DIRECTION('center_axis',(0.,-1.,0.));
#8329=DIRECTION('ref_axis',(1.,0.,0.));
#8330=DIRECTION('center_axis',(0.,-1.,0.));
#8331=DIRECTION('ref_axis',(1.,0.,0.));
#8332=DIRECTION('',(0.707106781186547,0.707106781186548,8.65956056235493E-17));
#8333=DIRECTION('center_axis',(0.,-1.,0.));
#8334=DIRECTION('ref_axis',(1.,0.,0.));
#8335=DIRECTION('center_axis',(0.,-1.,0.));
#8336=DIRECTION('ref_axis',(1.,0.,0.));
#8337=DIRECTION('',(0.,1.,0.));
#8338=DIRECTION('center_axis',(0.,1.,0.));
#8339=DIRECTION('ref_axis',(1.,0.,0.));
#8340=DIRECTION('center_axis',(0.,-1.,0.));
#8341=DIRECTION('ref_axis',(1.,0.,0.));
#8342=DIRECTION('',(-0.707106781186547,0.707106781186548,-8.65956056235493E-17));
#8343=DIRECTION('center_axis',(0.,-1.,0.));
#8344=DIRECTION('ref_axis',(0.,0.,-1.));
#8345=DIRECTION('center_axis',(0.,-1.,0.));
#8346=DIRECTION('ref_axis',(1.,0.,0.));
#8347=DIRECTION('center_axis',(0.,1.,0.));
#8348=DIRECTION('ref_axis',(1.,0.,0.));
#8349=DIRECTION('center_axis',(0.,1.,0.));
#8350=DIRECTION('ref_axis',(1.,0.,0.));
#8351=DIRECTION('',(-0.447213595499958,0.894427190999916,-5.47678698264203E-17));
#8352=DIRECTION('center_axis',(0.,-1.,0.));
#8353=DIRECTION('ref_axis',(1.,0.,0.));
#8354=DIRECTION('center_axis',(0.,1.,0.));
#8355=DIRECTION('ref_axis',(1.,0.,0.));
#8356=DIRECTION('',(0.,1.,0.));
#8357=DIRECTION('center_axis',(0.,1.,0.));
#8358=DIRECTION('ref_axis',(1.,0.,0.));
#8359=DIRECTION('center_axis',(0.,-1.,0.));
#8360=DIRECTION('ref_axis',(1.,0.,0.));
#8361=DIRECTION('',(-0.707106781186547,0.707106781186548,-8.65956056235493E-17));
#8362=DIRECTION('center_axis',(0.,-1.,0.));
#8363=DIRECTION('ref_axis',(0.,0.,-1.));
#8364=DIRECTION('center_axis',(0.866025403784439,0.,-0.5));
#8365=DIRECTION('ref_axis',(0.5,0.,0.866025403784439));
#8366=DIRECTION('',(-0.5,0.,-0.866025403784439));
#8367=DIRECTION('',(0.,-1.,0.));
#8368=DIRECTION('',(0.5,0.,0.866025403784439));
#8369=DIRECTION('',(0.,-1.,0.));
#8370=DIRECTION('center_axis',(1.60246890531964E-16,0.,-1.));
#8371=DIRECTION('ref_axis',(1.,0.,1.60246890531964E-16));
#8372=DIRECTION('',(-1.,0.,-1.60246890531964E-16));
#8373=DIRECTION('',(0.,-1.,0.));
#8374=DIRECTION('',(1.,0.,1.60246890531964E-16));
#8375=DIRECTION('center_axis',(-0.866025403784439,0.,-0.5));
#8376=DIRECTION('ref_axis',(0.5,0.,-0.866025403784439));
#8377=DIRECTION('',(-0.5,0.,0.866025403784439));
#8378=DIRECTION('',(0.,-1.,0.));
#8379=DIRECTION('',(0.5,0.,-0.866025403784439));
#8380=DIRECTION('center_axis',(-0.866025403784439,0.,0.5));
#8381=DIRECTION('ref_axis',(-0.5,0.,-0.866025403784439));
#8382=DIRECTION('',(0.5,0.,0.866025403784439));
#8383=DIRECTION('',(0.,-1.,0.));
#8384=DIRECTION('',(-0.5,0.,-0.866025403784439));
#8385=DIRECTION('center_axis',(-1.60246890531964E-16,0.,1.));
#8386=DIRECTION('ref_axis',(-1.,0.,-1.60246890531964E-16));
#8387=DIRECTION('',(1.,0.,1.60246890531964E-16));
#8388=DIRECTION('',(0.,-1.,0.));
#8389=DIRECTION('',(-1.,0.,-1.60246890531964E-16));
#8390=DIRECTION('center_axis',(0.866025403784439,0.,0.5));
#8391=DIRECTION('ref_axis',(-0.5,0.,0.866025403784439));
#8392=DIRECTION('',(0.5,0.,-0.866025403784439));
#8393=DIRECTION('',(-0.5,0.,0.866025403784439));
#8394=DIRECTION('center_axis',(0.,1.,0.));
#8395=DIRECTION('ref_axis',(1.,0.,0.));
#8396=DIRECTION('center_axis',(0.,-1.,0.));
#8397=DIRECTION('ref_axis',(0.,0.,-1.));
#8398=DIRECTION('axis',(0.,0.,1.));
#8399=DIRECTION('refdir',(1.,0.,0.));
#8400=DIRECTION('center_axis',(1.,0.,0.));
#8401=DIRECTION('ref_axis',(0.,0.,-1.));
#8402=DIRECTION('',(1.,0.,0.));
#8403=DIRECTION('center_axis',(0.,1.,0.));
#8404=DIRECTION('ref_axis',(0.,0.,1.));
#8405=DIRECTION('center_axis',(0.,-1.,0.));
#8406=DIRECTION('ref_axis',(1.,0.,0.));
#8407=DIRECTION('center_axis',(0.,-1.,0.));
#8408=DIRECTION('ref_axis',(1.,0.,0.));
#8409=DIRECTION('center_axis',(0.,-1.,0.));
#8410=DIRECTION('ref_axis',(1.,0.,0.));
#8411=DIRECTION('center_axis',(0.,-1.,0.));
#8412=DIRECTION('ref_axis',(1.,0.,0.));
#8413=DIRECTION('',(0.707106781186548,0.707106781186547,8.65956056235493E-17));
#8414=DIRECTION('center_axis',(0.,-1.,0.));
#8415=DIRECTION('ref_axis',(1.,0.,0.));
#8416=DIRECTION('center_axis',(0.,-1.,0.));
#8417=DIRECTION('ref_axis',(1.,0.,0.));
#8418=DIRECTION('',(0.,1.,0.));
#8419=DIRECTION('center_axis',(0.,1.,0.));
#8420=DIRECTION('ref_axis',(1.,0.,0.));
#8421=DIRECTION('center_axis',(0.,-1.,0.));
#8422=DIRECTION('ref_axis',(1.,0.,0.));
#8423=DIRECTION('',(-0.707106781186548,0.707106781186547,-8.65956056235494E-17));
#8424=DIRECTION('center_axis',(0.,-1.,0.));
#8425=DIRECTION('ref_axis',(0.,0.,-1.));
#8426=DIRECTION('center_axis',(0.,-1.,0.));
#8427=DIRECTION('ref_axis',(1.,0.,0.));
#8428=DIRECTION('center_axis',(0.,-1.,0.));
#8429=DIRECTION('ref_axis',(1.,0.,0.));
#8430=DIRECTION('',(0.,1.,0.));
#8431=DIRECTION('axis',(0.,0.,1.));
#8432=DIRECTION('refdir',(1.,0.,0.));
#8433=DIRECTION('axis',(0.,0.,1.));
#8434=DIRECTION('refdir',(1.,0.,0.));
#8435=DIRECTION('center_axis',(0.,0.,1.));
#8436=DIRECTION('ref_axis',(1.,0.,0.));
#8437=DIRECTION('',(0.,0.,1.));
#8438=DIRECTION('center_axis',(0.,1.,0.));
#8439=DIRECTION('ref_axis',(1.,0.,0.));
#8440=DIRECTION('center_axis',(0.,1.,0.));
#8441=DIRECTION('ref_axis',(1.,0.,0.));
#8442=DIRECTION('',(0.,1.,0.));
#8443=DIRECTION('center_axis',(0.,-1.,0.));
#8444=DIRECTION('ref_axis',(1.,0.,0.));
#8445=DIRECTION('center_axis',(-0.762527203906389,0.,0.646956152534856));
#8446=DIRECTION('ref_axis',(-0.646956152534856,0.,-0.762527203906389));
#8447=DIRECTION('',(0.646956152534856,0.,0.762527203906389));
#8448=DIRECTION('',(0.,-1.,0.));
#8449=DIRECTION('',(-0.646956152534856,0.,-0.762527203906389));
#8450=DIRECTION('',(0.,-1.,0.));
#8451=DIRECTION('center_axis',(-0.695442635009613,0.,0.718581617779697));
#8452=DIRECTION('ref_axis',(-0.718581617779697,0.,-0.695442635009613));
#8453=DIRECTION('',(0.718581617779697,0.,0.695442635009613));
#8454=DIRECTION('',(-0.718581617779697,0.,-0.695442635009613));
#8455=DIRECTION('',(0.,-1.,0.));
#8456=DIRECTION('center_axis',(-0.621660573370079,0.,0.783286749228649));
#8457=DIRECTION('ref_axis',(-0.783286749228649,0.,-0.621660573370079));
#8458=DIRECTION('',(0.783286749228649,0.,0.621660573370079));
#8459=DIRECTION('',(-0.783286749228649,0.,-0.621660573370079));
#8460=DIRECTION('',(0.,-1.,0.));
#8461=DIRECTION('center_axis',(-0.541891580574751,0.,0.840448401094439));
#8462=DIRECTION('ref_axis',(-0.840448401094439,0.,-0.541891580574751));
#8463=DIRECTION('',(0.840448401094439,0.,0.541891580574751));
#8464=DIRECTION('',(-0.840448401094439,0.,-0.541891580574751));
#8465=DIRECTION('',(0.,-1.,0.));
#8466=DIRECTION('center_axis',(-0.456903875630423,0.,0.889516075421855));
#8467=DIRECTION('ref_axis',(-0.889516075421855,0.,-0.456903875630423));
#8468=DIRECTION('',(0.889516075421855,0.,0.456903875630423));
#8469=DIRECTION('',(-0.889516075421855,0.,-0.456903875630423));
#8470=DIRECTION('',(0.,-1.,0.));
#8471=DIRECTION('center_axis',(-0.367515936594703,0.,0.930017223684012));
#8472=DIRECTION('ref_axis',(-0.930017223684012,0.,-0.367515936594703));
#8473=DIRECTION('',(0.930017223684012,0.,0.367515936594703));
#8474=DIRECTION('',(-0.930017223684012,0.,-0.367515936594703));
#8475=DIRECTION('',(0.,-1.,0.));
#8476=DIRECTION('center_axis',(-0.274588618184932,0.,0.961561797682962));
#8477=DIRECTION('ref_axis',(-0.961561797682962,0.,-0.274588618184932));
#8478=DIRECTION('',(0.961561797682962,0.,0.274588618184932));
#8479=DIRECTION('',(-0.961561797682962,0.,-0.274588618184932));
#8480=DIRECTION('',(0.,-1.,0.));
#8481=DIRECTION('center_axis',(-0.179016861276632,0.,0.983846005927077));
#8482=DIRECTION('ref_axis',(-0.983846005927077,0.,-0.179016861276632));
#8483=DIRECTION('',(0.983846005927077,0.,0.179016861276632));
#8484=DIRECTION('',(-0.983846005927077,0.,-0.179016861276632));
#8485=DIRECTION('',(0.,-1.,0.));
#8486=DIRECTION('center_axis',(0.99144486137381,0.,0.130526192220052));
#8487=DIRECTION('ref_axis',(-0.130526192220052,0.,0.99144486137381));
#8488=DIRECTION('',(0.130526192220052,0.,-0.99144486137381));
#8489=DIRECTION('',(-0.130526192220052,0.,0.99144486137381));
#8490=DIRECTION('',(0.,-1.,0.));
#8491=DIRECTION('center_axis',(0.179016861276633,0.,-0.983846005927077));
#8492=DIRECTION('ref_axis',(0.983846005927077,0.,0.179016861276633));
#8493=DIRECTION('',(-0.983846005927077,0.,-0.179016861276633));
#8494=DIRECTION('',(0.983846005927077,0.,0.179016861276633));
#8495=DIRECTION('',(0.,-1.,0.));
#8496=DIRECTION('center_axis',(0.274588618184932,0.,-0.961561797682962));
#8497=DIRECTION('ref_axis',(0.961561797682962,0.,0.274588618184932));
#8498=DIRECTION('',(-0.961561797682962,0.,-0.274588618184932));
#8499=DIRECTION('',(0.961561797682962,0.,0.274588618184932));
#8500=DIRECTION('',(0.,-1.,0.));
#8501=DIRECTION('center_axis',(0.367515936594704,0.,-0.930017223684012));
#8502=DIRECTION('ref_axis',(0.930017223684012,0.,0.367515936594704));
#8503=DIRECTION('',(-0.930017223684012,0.,-0.367515936594704));
#8504=DIRECTION('',(0.930017223684012,0.,0.367515936594704));
#8505=DIRECTION('',(0.,-1.,0.));
#8506=DIRECTION('center_axis',(0.456903875630421,0.,-0.889516075421856));
#8507=DIRECTION('ref_axis',(0.889516075421856,0.,0.456903875630421));
#8508=DIRECTION('',(-0.889516075421856,0.,-0.456903875630421));
#8509=DIRECTION('',(0.889516075421856,0.,0.456903875630421));
#8510=DIRECTION('',(0.,-1.,0.));
#8511=DIRECTION('center_axis',(0.541891580574752,0.,-0.840448401094438));
#8512=DIRECTION('ref_axis',(0.840448401094438,0.,0.541891580574752));
#8513=DIRECTION('',(-0.840448401094438,0.,-0.541891580574752));
#8514=DIRECTION('',(0.840448401094438,0.,0.541891580574752));
#8515=DIRECTION('',(0.,-1.,0.));
#8516=DIRECTION('center_axis',(0.621660573370078,0.,-0.78328674922865));
#8517=DIRECTION('ref_axis',(0.78328674922865,0.,0.621660573370078));
#8518=DIRECTION('',(-0.78328674922865,0.,-0.621660573370078));
#8519=DIRECTION('',(0.78328674922865,0.,0.621660573370078));
#8520=DIRECTION('',(0.,-1.,0.));
#8521=DIRECTION('center_axis',(0.695442635009612,0.,-0.718581617779697));
#8522=DIRECTION('ref_axis',(0.718581617779697,0.,0.695442635009612));
#8523=DIRECTION('',(-0.718581617779697,0.,-0.695442635009612));
#8524=DIRECTION('',(0.718581617779697,0.,0.695442635009612));
#8525=DIRECTION('',(0.,-1.,0.));
#8526=DIRECTION('center_axis',(0.762527203906389,0.,-0.646956152534857));
#8527=DIRECTION('ref_axis',(0.646956152534857,0.,0.762527203906389));
#8528=DIRECTION('',(-0.646956152534857,0.,-0.762527203906389));
#8529=DIRECTION('',(0.646956152534857,0.,0.762527203906389));
#8530=DIRECTION('',(0.,-1.,0.));
#8531=DIRECTION('center_axis',(-0.60876142900872,0.,-0.793353340291236));
#8532=DIRECTION('ref_axis',(0.793353340291236,0.,-0.60876142900872));
#8533=DIRECTION('',(-0.793353340291236,0.,0.60876142900872));
#8534=DIRECTION('',(0.793353340291236,0.,-0.60876142900872));
#8535=DIRECTION('center_axis',(0.,1.,0.));
#8536=DIRECTION('ref_axis',(-0.5,0.,0.866025403784438));
#8537=DIRECTION('center_axis',(0.,1.,0.));
#8538=DIRECTION('ref_axis',(1.,0.,0.));
#8539=DIRECTION('center_axis',(0.,1.,0.));
#8540=DIRECTION('ref_axis',(1.,0.,0.));
#8541=DIRECTION('center_axis',(0.,1.,0.));
#8542=DIRECTION('ref_axis',(1.,0.,0.));
#8543=DIRECTION('center_axis',(0.,1.,0.));
#8544=DIRECTION('ref_axis',(1.,0.,0.));
#8545=DIRECTION('center_axis',(0.,1.,0.));
#8546=DIRECTION('ref_axis',(1.,0.,0.));
#8547=DIRECTION('center_axis',(0.,1.,0.));
#8548=DIRECTION('ref_axis',(1.,0.,0.));
#8549=DIRECTION('center_axis',(0.,1.,0.));
#8550=DIRECTION('ref_axis',(1.,0.,0.));
#8551=DIRECTION('center_axis',(0.,1.,0.));
#8552=DIRECTION('ref_axis',(1.,0.,0.));
#8553=DIRECTION('center_axis',(0.,1.,0.));
#8554=DIRECTION('ref_axis',(1.,0.,0.));
#8555=DIRECTION('center_axis',(0.,1.,0.));
#8556=DIRECTION('ref_axis',(1.,0.,0.));
#8557=DIRECTION('center_axis',(0.,1.,0.));
#8558=DIRECTION('ref_axis',(1.,0.,0.));
#8559=DIRECTION('center_axis',(0.,1.,0.));
#8560=DIRECTION('ref_axis',(1.,0.,0.));
#8561=DIRECTION('center_axis',(0.,1.,0.));
#8562=DIRECTION('ref_axis',(1.,0.,0.));
#8563=DIRECTION('center_axis',(0.,1.,0.));
#8564=DIRECTION('ref_axis',(1.,0.,0.));
#8565=DIRECTION('center_axis',(0.,1.,0.));
#8566=DIRECTION('ref_axis',(1.,0.,0.));
#8567=DIRECTION('center_axis',(0.,1.,0.));
#8568=DIRECTION('ref_axis',(1.,0.,0.));
#8569=DIRECTION('center_axis',(0.,1.,0.));
#8570=DIRECTION('ref_axis',(1.,0.,0.));
#8571=DIRECTION('center_axis',(0.,1.,0.));
#8572=DIRECTION('ref_axis',(1.,0.,0.));
#8573=DIRECTION('',(-0.923879532511287,0.,-0.38268343236509));
#8574=DIRECTION('',(0.336889853392221,0.,-0.941544065183021));
#8575=DIRECTION('',(0.242980179903264,0.,-0.970031253194544));
#8576=DIRECTION('',(0.146730474455362,0.,-0.989176509964781));
#8577=DIRECTION('',(0.0490676743274181,0.,-0.998795456205172));
#8578=DIRECTION('',(-0.0490676743274181,0.,-0.998795456205172));
#8579=DIRECTION('',(-0.146730474455362,0.,-0.989176509964781));
#8580=DIRECTION('',(-0.242980179903264,0.,-0.970031253194544));
#8581=DIRECTION('',(-0.336889853392221,0.,-0.941544065183021));
#8582=DIRECTION('',(0.923879532511287,0.,-0.38268343236509));
#8583=DIRECTION('center_axis',(0.,1.,0.));
#8584=DIRECTION('ref_axis',(1.,0.,0.));
#8585=DIRECTION('',(0.130526192220051,0.,0.99144486137381));
#8586=DIRECTION('',(-0.983846005927078,0.,0.179016861276632));
#8587=DIRECTION('',(-0.961561797682962,0.,0.274588618184932));
#8588=DIRECTION('',(-0.930017223684012,0.,0.367515936594703));
#8589=DIRECTION('',(-0.889516075421856,0.,0.45690387563042));
#8590=DIRECTION('',(-0.840448401094438,0.,0.541891580574752));
#8591=DIRECTION('',(-0.78328674922865,0.,0.621660573370077));
#8592=DIRECTION('',(-0.718581617779698,0.,0.695442635009612));
#8593=DIRECTION('',(-0.646956152534857,0.,0.762527203906388));
#8594=DIRECTION('',(-0.793353340291235,0.,-0.608761429008721));
#8595=DIRECTION('center_axis',(0.,1.,0.));
#8596=DIRECTION('ref_axis',(1.,0.,0.));
#8597=DIRECTION('center_axis',(0.,1.,0.));
#8598=DIRECTION('ref_axis',(1.,0.,0.));
#8599=DIRECTION('center_axis',(-0.179016861276632,0.,-0.983846005927078));
#8600=DIRECTION('ref_axis',(0.983846005927078,0.,-0.179016861276632));
#8601=DIRECTION('',(-0.983846005927078,0.,0.179016861276632));
#8602=DIRECTION('',(0.,-1.,0.));
#8603=DIRECTION('',(0.983846005927078,0.,-0.179016861276632));
#8604=DIRECTION('',(0.,-1.,0.));
#8605=DIRECTION('center_axis',(-0.274588618184931,0.,-0.961561797682962));
#8606=DIRECTION('ref_axis',(0.961561797682962,0.,-0.274588618184931));
#8607=DIRECTION('',(-0.961561797682962,0.,0.274588618184931));
#8608=DIRECTION('',(0.961561797682962,0.,-0.274588618184931));
#8609=DIRECTION('',(0.,-1.,0.));
#8610=DIRECTION('center_axis',(-0.367515936594702,0.,-0.930017223684013));
#8611=DIRECTION('ref_axis',(0.930017223684013,0.,-0.367515936594702));
#8612=DIRECTION('',(-0.930017223684013,0.,0.367515936594703));
#8613=DIRECTION('',(0.930017223684013,0.,-0.367515936594702));
#8614=DIRECTION('',(0.,-1.,0.));
#8615=DIRECTION('center_axis',(-0.456903875630422,0.,-0.889516075421855));
#8616=DIRECTION('ref_axis',(0.889516075421855,0.,-0.456903875630422));
#8617=DIRECTION('',(-0.889516075421855,0.,0.456903875630422));
#8618=DIRECTION('',(0.889516075421855,0.,-0.456903875630422));
#8619=DIRECTION('',(0.,-1.,0.));
#8620=DIRECTION('center_axis',(-0.54189158057475,0.,-0.840448401094439));
#8621=DIRECTION('ref_axis',(0.840448401094439,0.,-0.54189158057475));
#8622=DIRECTION('',(-0.840448401094439,0.,0.54189158057475));
#8623=DIRECTION('',(0.840448401094439,0.,-0.54189158057475));
#8624=DIRECTION('',(0.,-1.,0.));
#8625=DIRECTION('center_axis',(-0.621660573370078,0.,-0.78328674922865));
#8626=DIRECTION('ref_axis',(0.78328674922865,0.,-0.621660573370078));
#8627=DIRECTION('',(-0.78328674922865,0.,0.621660573370078));
#8628=DIRECTION('',(0.78328674922865,0.,-0.621660573370078));
#8629=DIRECTION('',(0.,-1.,0.));
#8630=DIRECTION('center_axis',(-0.695442635009612,0.,-0.718581617779698));
#8631=DIRECTION('ref_axis',(0.718581617779698,0.,-0.695442635009612));
#8632=DIRECTION('',(-0.718581617779698,0.,0.695442635009612));
#8633=DIRECTION('',(0.718581617779698,0.,-0.695442635009612));
#8634=DIRECTION('',(0.,-1.,0.));
#8635=DIRECTION('center_axis',(-0.762527203906389,0.,-0.646956152534857));
#8636=DIRECTION('ref_axis',(0.646956152534857,0.,-0.762527203906389));
#8637=DIRECTION('',(-0.646956152534857,0.,0.762527203906389));
#8638=DIRECTION('',(0.646956152534857,0.,-0.762527203906389));
#8639=DIRECTION('',(0.,-1.,0.));
#8640=DIRECTION('center_axis',(-0.608761429008721,0.,0.793353340291235));
#8641=DIRECTION('ref_axis',(-0.793353340291235,0.,-0.608761429008721));
#8642=DIRECTION('',(0.793353340291235,0.,0.608761429008721));
#8643=DIRECTION('',(0.,-1.,0.));
#8644=DIRECTION('center_axis',(0.762527203906388,0.,0.646956152534857));
#8645=DIRECTION('ref_axis',(-0.646956152534857,0.,0.762527203906388));
#8646=DIRECTION('',(0.646956152534857,0.,-0.762527203906388));
#8647=DIRECTION('',(0.,-1.,0.));
#8648=DIRECTION('center_axis',(0.695442635009612,0.,0.718581617779698));
#8649=DIRECTION('ref_axis',(-0.718581617779698,0.,0.695442635009612));
#8650=DIRECTION('',(0.718581617779698,0.,-0.695442635009612));
#8651=DIRECTION('',(0.,-1.,0.));
#8652=DIRECTION('center_axis',(0.621660573370077,0.,0.78328674922865));
#8653=DIRECTION('ref_axis',(-0.78328674922865,0.,0.621660573370077));
#8654=DIRECTION('',(0.78328674922865,0.,-0.621660573370077));
#8655=DIRECTION('',(0.,-1.,0.));
#8656=DIRECTION('center_axis',(0.541891580574752,0.,0.840448401094438));
#8657=DIRECTION('ref_axis',(-0.840448401094438,0.,0.541891580574752));
#8658=DIRECTION('',(0.840448401094438,0.,-0.541891580574752));
#8659=DIRECTION('',(0.,-1.,0.));
#8660=DIRECTION('center_axis',(0.45690387563042,0.,0.889516075421856));
#8661=DIRECTION('ref_axis',(-0.889516075421856,0.,0.45690387563042));
#8662=DIRECTION('',(0.889516075421856,0.,-0.45690387563042));
#8663=DIRECTION('',(0.,-1.,0.));
#8664=DIRECTION('center_axis',(0.367515936594703,0.,0.930017223684012));
#8665=DIRECTION('ref_axis',(-0.930017223684012,0.,0.367515936594703));
#8666=DIRECTION('',(0.930017223684012,0.,-0.367515936594703));
#8667=DIRECTION('',(0.,-1.,0.));
#8668=DIRECTION('center_axis',(0.274588618184932,0.,0.961561797682962));
#8669=DIRECTION('ref_axis',(-0.961561797682962,0.,0.274588618184932));
#8670=DIRECTION('',(0.961561797682962,0.,-0.274588618184932));
#8671=DIRECTION('',(0.,-1.,0.));
#8672=DIRECTION('center_axis',(0.179016861276632,0.,0.983846005927078));
#8673=DIRECTION('ref_axis',(-0.983846005927078,0.,0.179016861276632));
#8674=DIRECTION('',(0.983846005927078,0.,-0.179016861276632));
#8675=DIRECTION('',(0.,-1.,0.));
#8676=DIRECTION('center_axis',(0.99144486137381,0.,-0.130526192220051));
#8677=DIRECTION('ref_axis',(0.130526192220051,0.,0.99144486137381));
#8678=DIRECTION('',(-0.130526192220051,0.,-0.99144486137381));
#8679=DIRECTION('center_axis',(0.,1.,0.));
#8680=DIRECTION('ref_axis',(-0.5,0.,-0.866025403784439));
#8681=DIRECTION('center_axis',(0.,1.,0.));
#8682=DIRECTION('ref_axis',(1.,0.,0.));
#8683=DIRECTION('center_axis',(0.,1.,0.));
#8684=DIRECTION('ref_axis',(1.,0.,0.));
#8685=DIRECTION('center_axis',(0.,1.,0.));
#8686=DIRECTION('ref_axis',(1.,0.,0.));
#8687=DIRECTION('center_axis',(0.,1.,0.));
#8688=DIRECTION('ref_axis',(1.,0.,0.));
#8689=DIRECTION('center_axis',(0.,1.,0.));
#8690=DIRECTION('ref_axis',(1.,0.,0.));
#8691=DIRECTION('center_axis',(0.,1.,0.));
#8692=DIRECTION('ref_axis',(1.,0.,0.));
#8693=DIRECTION('center_axis',(0.,1.,0.));
#8694=DIRECTION('ref_axis',(1.,0.,0.));
#8695=DIRECTION('center_axis',(0.,1.,0.));
#8696=DIRECTION('ref_axis',(1.,0.,0.));
#8697=DIRECTION('center_axis',(0.,1.,0.));
#8698=DIRECTION('ref_axis',(1.,0.,0.));
#8699=DIRECTION('center_axis',(0.,1.,0.));
#8700=DIRECTION('ref_axis',(1.,0.,0.));
#8701=DIRECTION('center_axis',(0.,1.,0.));
#8702=DIRECTION('ref_axis',(1.,0.,0.));
#8703=DIRECTION('center_axis',(0.,1.,0.));
#8704=DIRECTION('ref_axis',(1.,0.,0.));
#8705=DIRECTION('center_axis',(0.,1.,0.));
#8706=DIRECTION('ref_axis',(1.,0.,0.));
#8707=DIRECTION('center_axis',(0.,1.,0.));
#8708=DIRECTION('ref_axis',(1.,0.,0.));
#8709=DIRECTION('center_axis',(0.,1.,0.));
#8710=DIRECTION('ref_axis',(1.,0.,0.));
#8711=DIRECTION('center_axis',(0.,1.,0.));
#8712=DIRECTION('ref_axis',(1.,0.,0.));
#8713=DIRECTION('center_axis',(0.94154406518302,0.,0.336889853392221));
#8714=DIRECTION('ref_axis',(-0.336889853392221,0.,0.94154406518302));
#8715=DIRECTION('',(0.336889853392221,0.,-0.94154406518302));
#8716=DIRECTION('',(0.,-1.,0.));
#8717=DIRECTION('',(-0.336889853392221,0.,0.94154406518302));
#8718=DIRECTION('',(0.,-1.,0.));
#8719=DIRECTION('center_axis',(0.970031253194544,0.,0.242980179903265));
#8720=DIRECTION('ref_axis',(-0.242980179903265,0.,0.970031253194544));
#8721=DIRECTION('',(0.242980179903265,0.,-0.970031253194544));
#8722=DIRECTION('',(-0.242980179903265,0.,0.970031253194544));
#8723=DIRECTION('',(0.,-1.,0.));
#8724=DIRECTION('center_axis',(0.989176509964781,0.,0.146730474455363));
#8725=DIRECTION('ref_axis',(-0.146730474455363,0.,0.989176509964781));
#8726=DIRECTION('',(0.146730474455363,0.,-0.989176509964781));
#8727=DIRECTION('',(-0.146730474455363,0.,0.989176509964781));
#8728=DIRECTION('',(0.,-1.,0.));
#8729=DIRECTION('center_axis',(0.998795456205173,0.,0.049067674327416));
#8730=DIRECTION('ref_axis',(-0.049067674327416,0.,0.998795456205173));
#8731=DIRECTION('',(0.049067674327416,0.,-0.998795456205173));
#8732=DIRECTION('',(-0.049067674327416,0.,0.998795456205173));
#8733=DIRECTION('',(0.,-1.,0.));
#8734=DIRECTION('center_axis',(0.998795456205173,0.,-0.049067674327416));
#8735=DIRECTION('ref_axis',(0.049067674327416,0.,0.998795456205173));
#8736=DIRECTION('',(-0.049067674327416,0.,-0.998795456205173));
#8737=DIRECTION('',(0.049067674327416,0.,0.998795456205173));
#8738=DIRECTION('',(0.,-1.,0.));
#8739=DIRECTION('center_axis',(0.989176509964781,0.,-0.146730474455363));
#8740=DIRECTION('ref_axis',(0.146730474455363,0.,0.989176509964781));
#8741=DIRECTION('',(-0.146730474455363,0.,-0.989176509964781));
#8742=DIRECTION('',(0.146730474455363,0.,0.989176509964781));
#8743=DIRECTION('',(0.,-1.,0.));
#8744=DIRECTION('center_axis',(0.970031253194544,0.,-0.242980179903265));
#8745=DIRECTION('ref_axis',(0.242980179903265,0.,0.970031253194544));
#8746=DIRECTION('',(-0.242980179903265,0.,-0.970031253194544));
#8747=DIRECTION('',(0.242980179903265,0.,0.970031253194544));
#8748=DIRECTION('',(0.,-1.,0.));
#8749=DIRECTION('center_axis',(0.94154406518302,0.,-0.336889853392221));
#8750=DIRECTION('ref_axis',(0.336889853392221,0.,0.94154406518302));
#8751=DIRECTION('',(-0.336889853392221,0.,-0.94154406518302));
#8752=DIRECTION('',(0.336889853392221,0.,0.94154406518302));
#8753=DIRECTION('',(0.,-1.,0.));
#8754=DIRECTION('center_axis',(-0.38268343236509,0.,-0.923879532511287));
#8755=DIRECTION('ref_axis',(0.923879532511287,0.,-0.38268343236509));
#8756=DIRECTION('',(-0.923879532511287,0.,0.38268343236509));
#8757=DIRECTION('',(0.,-1.,0.));
#8758=DIRECTION('center_axis',(-0.941544065183021,0.,0.336889853392221));
#8759=DIRECTION('ref_axis',(-0.336889853392221,0.,-0.941544065183021));
#8760=DIRECTION('',(0.336889853392221,0.,0.941544065183021));
#8761=DIRECTION('',(0.,-1.,0.));
#8762=DIRECTION('center_axis',(-0.970031253194544,0.,0.242980179903264));
#8763=DIRECTION('ref_axis',(-0.242980179903264,0.,-0.970031253194544));
#8764=DIRECTION('',(0.242980179903264,0.,0.970031253194544));
#8765=DIRECTION('',(0.,-1.,0.));
#8766=DIRECTION('center_axis',(-0.989176509964781,0.,0.146730474455362));
#8767=DIRECTION('ref_axis',(-0.146730474455362,0.,-0.989176509964781));
#8768=DIRECTION('',(0.146730474455362,0.,0.989176509964781));
#8769=DIRECTION('',(0.,-1.,0.));
#8770=DIRECTION('center_axis',(-0.998795456205172,0.,0.0490676743274181));
#8771=DIRECTION('ref_axis',(-0.0490676743274181,0.,-0.998795456205172));
#8772=DIRECTION('',(0.0490676743274181,0.,0.998795456205172));
#8773=DIRECTION('',(0.,-1.,0.));
#8774=DIRECTION('center_axis',(-0.998795456205172,0.,-0.0490676743274181));
#8775=DIRECTION('ref_axis',(0.0490676743274181,0.,-0.998795456205172));
#8776=DIRECTION('',(-0.0490676743274181,0.,0.998795456205172));
#8777=DIRECTION('',(0.,-1.,0.));
#8778=DIRECTION('center_axis',(-0.989176509964781,0.,-0.146730474455362));
#8779=DIRECTION('ref_axis',(0.146730474455362,0.,-0.989176509964781));
#8780=DIRECTION('',(-0.146730474455362,0.,0.989176509964781));
#8781=DIRECTION('',(0.,-1.,0.));
#8782=DIRECTION('center_axis',(-0.970031253194544,0.,-0.242980179903264));
#8783=DIRECTION('ref_axis',(0.242980179903264,0.,-0.970031253194544));
#8784=DIRECTION('',(-0.242980179903264,0.,0.970031253194544));
#8785=DIRECTION('',(0.,-1.,0.));
#8786=DIRECTION('center_axis',(-0.941544065183021,0.,-0.336889853392221));
#8787=DIRECTION('ref_axis',(0.336889853392221,0.,-0.941544065183021));
#8788=DIRECTION('',(-0.336889853392221,0.,0.941544065183021));
#8789=DIRECTION('',(0.,-1.,0.));
#8790=DIRECTION('center_axis',(-0.38268343236509,0.,0.923879532511287));
#8791=DIRECTION('ref_axis',(-0.923879532511287,0.,-0.38268343236509));
#8792=DIRECTION('',(0.923879532511287,0.,0.38268343236509));
#8793=DIRECTION('center_axis',(0.,1.,0.));
#8794=DIRECTION('ref_axis',(1.,0.,0.));
#8795=DIRECTION('center_axis',(0.,1.,0.));
#8796=DIRECTION('ref_axis',(1.,0.,0.));
#8797=DIRECTION('center_axis',(0.,1.,0.));
#8798=DIRECTION('ref_axis',(1.,0.,0.));
#8799=DIRECTION('center_axis',(0.,1.,0.));
#8800=DIRECTION('ref_axis',(1.,0.,0.));
#8801=DIRECTION('center_axis',(0.,1.,0.));
#8802=DIRECTION('ref_axis',(1.,0.,0.));
#8803=DIRECTION('center_axis',(0.,1.,0.));
#8804=DIRECTION('ref_axis',(1.,0.,0.));
#8805=DIRECTION('center_axis',(0.,1.,0.));
#8806=DIRECTION('ref_axis',(1.,0.,0.));
#8807=DIRECTION('center_axis',(0.,1.,0.));
#8808=DIRECTION('ref_axis',(1.,0.,0.));
#8809=DIRECTION('center_axis',(0.,1.,0.));
#8810=DIRECTION('ref_axis',(1.,0.,0.));
#8811=DIRECTION('center_axis',(0.,1.,0.));
#8812=DIRECTION('ref_axis',(1.,0.,0.));
#8813=DIRECTION('center_axis',(0.,1.,0.));
#8814=DIRECTION('ref_axis',(1.,0.,0.));
#8815=DIRECTION('center_axis',(0.,1.,0.));
#8816=DIRECTION('ref_axis',(1.,0.,0.));
#8817=DIRECTION('center_axis',(0.,1.,0.));
#8818=DIRECTION('ref_axis',(1.,0.,0.));
#8819=DIRECTION('center_axis',(0.,1.,0.));
#8820=DIRECTION('ref_axis',(1.,0.,0.));
#8821=DIRECTION('center_axis',(0.,1.,0.));
#8822=DIRECTION('ref_axis',(1.,0.,0.));
#8823=DIRECTION('center_axis',(0.,1.,0.));
#8824=DIRECTION('ref_axis',(1.,0.,0.));
#8825=DIRECTION('center_axis',(0.,1.,0.));
#8826=DIRECTION('ref_axis',(1.,0.,0.));
#8827=DIRECTION('center_axis',(0.,-1.,0.));
#8828=DIRECTION('ref_axis',(1.,0.,0.));
#8829=DIRECTION('center_axis',(0.,-1.,0.));
#8830=DIRECTION('ref_axis',(1.,0.,0.));
#8831=DIRECTION('',(0.,1.,0.));
#8832=DIRECTION('center_axis',(0.,1.,0.));
#8833=DIRECTION('ref_axis',(1.,0.,0.));
#8834=DIRECTION('axis',(0.,0.,1.));
#8835=DIRECTION('refdir',(1.,0.,0.));
#8836=DIRECTION('center_axis',(0.866025403784439,0.,0.5));
#8837=DIRECTION('ref_axis',(0.5,0.,-0.866025403784439));
#8838=DIRECTION('',(0.866025403784439,0.,0.5));
#8839=DIRECTION('center_axis',(0.,1.,0.));
#8840=DIRECTION('ref_axis',(0.5,0.,-0.866025403784439));
#8841=DIRECTION('center_axis',(0.,1.,0.));
#8842=DIRECTION('ref_axis',(0.5,0.,-0.866025403784439));
#8843=DIRECTION('',(0.,1.,0.));
#8844=DIRECTION('center_axis',(0.,-1.,0.));
#8845=DIRECTION('ref_axis',(0.5,0.,-0.866025403784439));
#8846=DIRECTION('center_axis',(-0.179016861276632,0.,-0.983846005927078));
#8847=DIRECTION('ref_axis',(-0.983846005927078,0.,0.179016861276632));
#8848=DIRECTION('',(-0.983846005927078,0.,0.179016861276632));
#8849=DIRECTION('',(0.,1.,0.));
#8850=DIRECTION('',(-0.983846005927078,0.,0.179016861276632));
#8851=DIRECTION('',(0.,1.,0.));
#8852=DIRECTION('center_axis',(-0.274588618184931,0.,-0.961561797682962));
#8853=DIRECTION('ref_axis',(-0.961561797682962,0.,0.274588618184931));
#8854=DIRECTION('',(-0.961561797682962,0.,0.274588618184931));
#8855=DIRECTION('',(-0.961561797682962,0.,0.274588618184931));
#8856=DIRECTION('',(0.,1.,0.));
#8857=DIRECTION('center_axis',(-0.367515936594703,0.,-0.930017223684013));
#8858=DIRECTION('ref_axis',(-0.930017223684012,0.,0.367515936594703));
#8859=DIRECTION('',(-0.930017223684012,0.,0.367515936594703));
#8860=DIRECTION('',(-0.930017223684013,0.,0.367515936594703));
#8861=DIRECTION('',(0.,1.,0.));
#8862=DIRECTION('center_axis',(-0.45690387563042,0.,-0.889516075421857));
#8863=DIRECTION('ref_axis',(-0.889516075421857,0.,0.45690387563042));
#8864=DIRECTION('',(-0.889516075421857,0.,0.45690387563042));
#8865=DIRECTION('',(-0.889516075421857,0.,0.45690387563042));
#8866=DIRECTION('',(0.,1.,0.));
#8867=DIRECTION('center_axis',(-0.541891580574751,0.,-0.840448401094438));
#8868=DIRECTION('ref_axis',(-0.840448401094438,0.,0.541891580574751));
#8869=DIRECTION('',(-0.840448401094438,0.,0.541891580574751));
#8870=DIRECTION('',(-0.840448401094438,0.,0.541891580574751));
#8871=DIRECTION('',(0.,1.,0.));
#8872=DIRECTION('center_axis',(-0.621660573370077,0.,-0.783286749228651));
#8873=DIRECTION('ref_axis',(-0.783286749228651,0.,0.621660573370077));
#8874=DIRECTION('',(-0.783286749228651,0.,0.621660573370077));
#8875=DIRECTION('',(-0.783286749228651,0.,0.621660573370077));
#8876=DIRECTION('',(0.,1.,0.));
#8877=DIRECTION('center_axis',(-0.695442635009612,0.,-0.718581617779698));
#8878=DIRECTION('ref_axis',(-0.718581617779698,0.,0.695442635009612));
#8879=DIRECTION('',(-0.718581617779698,0.,0.695442635009612));
#8880=DIRECTION('',(-0.718581617779698,0.,0.695442635009612));
#8881=DIRECTION('',(0.,1.,0.));
#8882=DIRECTION('center_axis',(-0.762527203906388,0.,-0.646956152534857));
#8883=DIRECTION('ref_axis',(-0.646956152534857,0.,0.762527203906388));
#8884=DIRECTION('',(-0.646956152534858,0.,0.762527203906388));
#8885=DIRECTION('',(-0.646956152534857,0.,0.762527203906388));
#8886=DIRECTION('',(0.,1.,0.));
#8887=DIRECTION('center_axis',(0.608761429008721,0.,-0.793353340291235));
#8888=DIRECTION('ref_axis',(-0.793353340291235,0.,-0.608761429008721));
#8889=DIRECTION('',(-0.793353340291235,0.,-0.608761429008721));
#8890=DIRECTION('',(-0.793353340291235,0.,-0.608761429008721));
#8891=DIRECTION('',(0.,1.,0.));
#8892=DIRECTION('center_axis',(0.762527203906388,0.,0.646956152534857));
#8893=DIRECTION('ref_axis',(0.646956152534857,0.,-0.762527203906388));
#8894=DIRECTION('',(0.646956152534857,0.,-0.762527203906388));
#8895=DIRECTION('',(0.646956152534857,0.,-0.762527203906388));
#8896=DIRECTION('',(0.,1.,0.));
#8897=DIRECTION('center_axis',(0.695442635009612,0.,0.718581617779698));
#8898=DIRECTION('ref_axis',(0.718581617779698,0.,-0.695442635009612));
#8899=DIRECTION('',(0.718581617779698,0.,-0.695442635009612));
#8900=DIRECTION('',(0.718581617779698,0.,-0.695442635009612));
#8901=DIRECTION('',(0.,1.,0.));
#8902=DIRECTION('center_axis',(0.621660573370078,0.,0.78328674922865));
#8903=DIRECTION('ref_axis',(0.78328674922865,0.,-0.621660573370078));
#8904=DIRECTION('',(0.78328674922865,0.,-0.621660573370078));
#8905=DIRECTION('',(0.78328674922865,0.,-0.621660573370078));
#8906=DIRECTION('',(0.,1.,0.));
#8907=DIRECTION('center_axis',(0.54189158057475,0.,0.84044840109444));
#8908=DIRECTION('ref_axis',(0.84044840109444,0.,-0.54189158057475));
#8909=DIRECTION('',(0.84044840109444,0.,-0.54189158057475));
#8910=DIRECTION('',(0.84044840109444,0.,-0.54189158057475));
#8911=DIRECTION('',(0.,1.,0.));
#8912=DIRECTION('center_axis',(0.456903875630422,0.,0.889516075421856));
#8913=DIRECTION('ref_axis',(0.889516075421856,0.,-0.456903875630422));
#8914=DIRECTION('',(0.889516075421856,0.,-0.456903875630422));
#8915=DIRECTION('',(0.889516075421856,0.,-0.456903875630422));
#8916=DIRECTION('',(0.,1.,0.));
#8917=DIRECTION('center_axis',(0.367515936594702,0.,0.930017223684013));
#8918=DIRECTION('ref_axis',(0.930017223684013,0.,-0.367515936594702));
#8919=DIRECTION('',(0.930017223684013,0.,-0.367515936594702));
#8920=DIRECTION('',(0.930017223684013,0.,-0.367515936594702));
#8921=DIRECTION('',(0.,1.,0.));
#8922=DIRECTION('center_axis',(0.274588618184931,0.,0.961561797682962));
#8923=DIRECTION('ref_axis',(0.961561797682962,0.,-0.274588618184931));
#8924=DIRECTION('',(0.961561797682962,0.,-0.274588618184931));
#8925=DIRECTION('',(0.961561797682962,0.,-0.274588618184931));
#8926=DIRECTION('',(0.,1.,0.));
#8927=DIRECTION('center_axis',(0.179016861276631,0.,0.983846005927078));
#8928=DIRECTION('ref_axis',(0.983846005927078,0.,-0.179016861276631));
#8929=DIRECTION('',(0.983846005927078,0.,-0.179016861276631));
#8930=DIRECTION('',(0.983846005927078,0.,-0.179016861276631));
#8931=DIRECTION('',(0.,1.,0.));
#8932=DIRECTION('center_axis',(-0.99144486137381,0.,0.130526192220051));
#8933=DIRECTION('ref_axis',(0.130526192220051,0.,0.99144486137381));
#8934=DIRECTION('',(0.130526192220051,0.,0.99144486137381));
#8935=DIRECTION('',(0.130526192220051,0.,0.99144486137381));
#8936=DIRECTION('center_axis',(0.,1.,0.));
#8937=DIRECTION('ref_axis',(0.499999999999999,0.,0.866025403784439));
#8938=DIRECTION('center_axis',(0.,1.,0.));
#8939=DIRECTION('ref_axis',(0.5,0.,-0.866025403784439));
#8940=DIRECTION('center_axis',(0.,1.,0.));
#8941=DIRECTION('ref_axis',(0.5,0.,-0.866025403784438));
#8942=DIRECTION('center_axis',(0.,1.,0.));
#8943=DIRECTION('ref_axis',(0.5,0.,-0.866025403784439));
#8944=DIRECTION('center_axis',(0.,1.,0.));
#8945=DIRECTION('ref_axis',(0.5,0.,-0.866025403784438));
#8946=DIRECTION('center_axis',(0.,1.,0.));
#8947=DIRECTION('ref_axis',(0.5,0.,-0.866025403784439));
#8948=DIRECTION('center_axis',(0.,1.,0.));
#8949=DIRECTION('ref_axis',(0.5,0.,-0.866025403784438));
#8950=DIRECTION('center_axis',(0.,1.,0.));
#8951=DIRECTION('ref_axis',(0.5,0.,-0.866025403784439));
#8952=DIRECTION('center_axis',(0.,1.,0.));
#8953=DIRECTION('ref_axis',(0.5,0.,-0.866025403784438));
#8954=DIRECTION('center_axis',(0.,1.,0.));
#8955=DIRECTION('ref_axis',(0.5,0.,-0.866025403784439));
#8956=DIRECTION('center_axis',(0.,1.,0.));
#8957=DIRECTION('ref_axis',(0.5,0.,-0.866025403784438));
#8958=DIRECTION('center_axis',(0.,1.,0.));
#8959=DIRECTION('ref_axis',(0.5,0.,-0.866025403784439));
#8960=DIRECTION('center_axis',(0.,1.,0.));
#8961=DIRECTION('ref_axis',(0.5,0.,-0.866025403784438));
#8962=DIRECTION('center_axis',(0.,1.,0.));
#8963=DIRECTION('ref_axis',(0.5,0.,-0.866025403784439));
#8964=DIRECTION('center_axis',(0.,1.,0.));
#8965=DIRECTION('ref_axis',(0.5,0.,-0.866025403784438));
#8966=DIRECTION('center_axis',(0.,1.,0.));
#8967=DIRECTION('ref_axis',(0.5,0.,-0.866025403784438));
#8968=DIRECTION('',(0.923879532511287,0.,-0.38268343236509));
#8969=DIRECTION('',(-0.33688985339222,0.,-0.941544065183021));
#8970=DIRECTION('',(-0.242980179903264,0.,-0.970031253194544));
#8971=DIRECTION('',(-0.146730474455362,0.,-0.989176509964781));
#8972=DIRECTION('',(-0.0490676743274178,0.,-0.998795456205172));
#8973=DIRECTION('',(0.0490676743274185,0.,-0.998795456205172));
#8974=DIRECTION('',(0.146730474455362,0.,-0.989176509964781));
#8975=DIRECTION('',(0.242980179903265,0.,-0.970031253194544));
#8976=DIRECTION('',(0.336889853392221,0.,-0.941544065183021));
#8977=DIRECTION('',(-0.923879532511287,0.,-0.38268343236509));
#8978=DIRECTION('center_axis',(0.,1.,0.));
#8979=DIRECTION('ref_axis',(0.5,0.,-0.866025403784438));
#8980=DIRECTION('',(-0.130526192220052,0.,0.99144486137381));
#8981=DIRECTION('',(0.983846005927078,0.,0.179016861276632));
#8982=DIRECTION('',(0.961561797682962,0.,0.274588618184932));
#8983=DIRECTION('',(0.930017223684012,0.,0.367515936594704));
#8984=DIRECTION('',(0.889516075421856,0.,0.456903875630421));
#8985=DIRECTION('',(0.840448401094438,0.,0.541891580574752));
#8986=DIRECTION('',(0.78328674922865,0.,0.621660573370078));
#8987=DIRECTION('',(0.718581617779698,0.,0.695442635009612));
#8988=DIRECTION('',(0.646956152534857,0.,0.762527203906389));
#8989=DIRECTION('',(0.793353340291235,0.,-0.60876142900872));
#8990=DIRECTION('center_axis',(0.,1.,0.));
#8991=DIRECTION('ref_axis',(0.5,0.,-0.866025403784438));
#8992=DIRECTION('center_axis',(0.,1.,0.));
#8993=DIRECTION('ref_axis',(0.5,0.,-0.866025403784439));
#8994=DIRECTION('center_axis',(0.,1.,0.));
#8995=DIRECTION('ref_axis',(0.5,0.,-0.866025403784438));
#8996=DIRECTION('center_axis',(0.,1.,0.));
#8997=DIRECTION('ref_axis',(0.5,0.,-0.866025403784439));
#8998=DIRECTION('center_axis',(0.,1.,0.));
#8999=DIRECTION('ref_axis',(0.5,0.,-0.866025403784438));
#9000=DIRECTION('center_axis',(0.941544065183021,0.,0.336889853392221));
#9001=DIRECTION('ref_axis',(0.336889853392221,0.,-0.941544065183021));
#9002=DIRECTION('',(0.336889853392221,0.,-0.941544065183021));
#9003=DIRECTION('',(0.,1.,0.));
#9004=DIRECTION('',(0.,1.,0.));
#9005=DIRECTION('center_axis',(0.970031253194544,0.,0.242980179903265));
#9006=DIRECTION('ref_axis',(0.242980179903265,0.,-0.970031253194544));
#9007=DIRECTION('',(0.242980179903265,0.,-0.970031253194544));
#9008=DIRECTION('',(0.,1.,0.));
#9009=DIRECTION('center_axis',(0.989176509964781,0.,0.146730474455362));
#9010=DIRECTION('ref_axis',(0.146730474455362,0.,-0.989176509964781));
#9011=DIRECTION('',(0.146730474455362,0.,-0.989176509964781));
#9012=DIRECTION('',(0.,1.,0.));
#9013=DIRECTION('center_axis',(0.998795456205172,0.,0.0490676743274185));
#9014=DIRECTION('ref_axis',(0.0490676743274185,0.,-0.998795456205172));
#9015=DIRECTION('',(0.0490676743274185,0.,-0.998795456205172));
#9016=DIRECTION('',(0.,1.,0.));
#9017=DIRECTION('center_axis',(0.998795456205172,0.,-0.0490676743274178));
#9018=DIRECTION('ref_axis',(-0.0490676743274178,0.,-0.998795456205172));
#9019=DIRECTION('',(-0.0490676743274178,0.,-0.998795456205172));
#9020=DIRECTION('',(0.,1.,0.));
#9021=DIRECTION('center_axis',(0.989176509964781,0.,-0.146730474455361));
#9022=DIRECTION('ref_axis',(-0.146730474455361,0.,-0.989176509964781));
#9023=DIRECTION('',(-0.146730474455361,0.,-0.989176509964781));
#9024=DIRECTION('',(0.,1.,0.));
#9025=DIRECTION('center_axis',(0.970031253194544,0.,-0.242980179903264));
#9026=DIRECTION('ref_axis',(-0.242980179903264,0.,-0.970031253194544));
#9027=DIRECTION('',(-0.242980179903264,0.,-0.970031253194544));
#9028=DIRECTION('',(0.,1.,0.));
#9029=DIRECTION('center_axis',(0.941544065183021,0.,-0.33688985339222));
#9030=DIRECTION('ref_axis',(-0.33688985339222,0.,-0.941544065183021));
#9031=DIRECTION('',(-0.33688985339222,0.,-0.941544065183021));
#9032=DIRECTION('',(0.,1.,0.));
#9033=DIRECTION('center_axis',(0.38268343236509,0.,0.923879532511287));
#9034=DIRECTION('ref_axis',(0.923879532511287,0.,-0.38268343236509));
#9035=DIRECTION('',(0.923879532511287,0.,-0.38268343236509));
#9036=DIRECTION('',(0.,1.,0.));
#9037=DIRECTION('center_axis',(-0.941544065183021,0.,0.336889853392221));
#9038=DIRECTION('ref_axis',(0.336889853392221,0.,0.941544065183021));
#9039=DIRECTION('',(0.336889853392221,0.,0.941544065183021));
#9040=DIRECTION('',(0.336889853392221,0.,0.941544065183021));
#9041=DIRECTION('',(0.,1.,0.));
#9042=DIRECTION('center_axis',(-0.970031253194544,0.,0.242980179903264));
#9043=DIRECTION('ref_axis',(0.242980179903264,0.,0.970031253194544));
#9044=DIRECTION('',(0.242980179903264,0.,0.970031253194544));
#9045=DIRECTION('',(0.242980179903264,0.,0.970031253194544));
#9046=DIRECTION('',(0.,1.,0.));
#9047=DIRECTION('center_axis',(-0.989176509964781,0.,0.146730474455362));
#9048=DIRECTION('ref_axis',(0.146730474455362,0.,0.989176509964781));
#9049=DIRECTION('',(0.146730474455362,0.,0.989176509964781));
#9050=DIRECTION('',(0.146730474455362,0.,0.989176509964781));
#9051=DIRECTION('',(0.,1.,0.));
#9052=DIRECTION('center_axis',(-0.998795456205173,0.,0.0490676743274157));
#9053=DIRECTION('ref_axis',(0.0490676743274157,0.,0.998795456205173));
#9054=DIRECTION('',(0.0490676743274157,0.,0.998795456205173));
#9055=DIRECTION('',(0.0490676743274157,0.,0.998795456205173));
#9056=DIRECTION('',(0.,1.,0.));
#9057=DIRECTION('center_axis',(-0.998795456205173,0.,-0.0490676743274162));
#9058=DIRECTION('ref_axis',(-0.0490676743274162,0.,0.998795456205173));
#9059=DIRECTION('',(-0.0490676743274162,0.,0.998795456205173));
#9060=DIRECTION('',(-0.0490676743274162,0.,0.998795456205173));
#9061=DIRECTION('',(0.,1.,0.));
#9062=DIRECTION('center_axis',(-0.989176509964781,0.,-0.146730474455363));
#9063=DIRECTION('ref_axis',(-0.146730474455363,0.,0.989176509964781));
#9064=DIRECTION('',(-0.146730474455363,0.,0.989176509964781));
#9065=DIRECTION('',(-0.146730474455363,0.,0.989176509964781));
#9066=DIRECTION('',(0.,1.,0.));
#9067=DIRECTION('center_axis',(-0.970031253194544,0.,-0.242980179903265));
#9068=DIRECTION('ref_axis',(-0.242980179903265,0.,0.970031253194544));
#9069=DIRECTION('',(-0.242980179903265,0.,0.970031253194544));
#9070=DIRECTION('',(-0.242980179903265,0.,0.970031253194544));
#9071=DIRECTION('',(0.,1.,0.));
#9072=DIRECTION('center_axis',(-0.94154406518302,0.,-0.336889853392221));
#9073=DIRECTION('ref_axis',(-0.336889853392221,0.,0.94154406518302));
#9074=DIRECTION('',(-0.336889853392221,0.,0.94154406518302));
#9075=DIRECTION('',(-0.336889853392221,0.,0.94154406518302));
#9076=DIRECTION('',(0.,1.,0.));
#9077=DIRECTION('center_axis',(0.38268343236509,0.,-0.923879532511287));
#9078=DIRECTION('ref_axis',(-0.923879532511287,0.,-0.38268343236509));
#9079=DIRECTION('',(-0.923879532511287,0.,-0.38268343236509));
#9080=DIRECTION('center_axis',(0.,1.,0.));
#9081=DIRECTION('ref_axis',(-1.,0.,-3.33066907387547E-16));
#9082=DIRECTION('center_axis',(0.,1.,0.));
#9083=DIRECTION('ref_axis',(0.5,0.,-0.866025403784439));
#9084=DIRECTION('center_axis',(0.,1.,0.));
#9085=DIRECTION('ref_axis',(0.5,0.,-0.866025403784438));
#9086=DIRECTION('center_axis',(0.,1.,0.));
#9087=DIRECTION('ref_axis',(0.5,0.,-0.866025403784439));
#9088=DIRECTION('center_axis',(0.,1.,0.));
#9089=DIRECTION('ref_axis',(0.5,0.,-0.866025403784438));
#9090=DIRECTION('center_axis',(0.,1.,0.));
#9091=DIRECTION('ref_axis',(0.5,0.,-0.866025403784439));
#9092=DIRECTION('center_axis',(0.,1.,0.));
#9093=DIRECTION('ref_axis',(0.5,0.,-0.866025403784438));
#9094=DIRECTION('center_axis',(0.,1.,0.));
#9095=DIRECTION('ref_axis',(0.5,0.,-0.866025403784439));
#9096=DIRECTION('center_axis',(0.,1.,0.));
#9097=DIRECTION('ref_axis',(0.5,0.,-0.866025403784438));
#9098=DIRECTION('center_axis',(0.,1.,0.));
#9099=DIRECTION('ref_axis',(0.5,0.,-0.866025403784439));
#9100=DIRECTION('center_axis',(0.,1.,0.));
#9101=DIRECTION('ref_axis',(0.5,0.,-0.866025403784438));
#9102=DIRECTION('center_axis',(0.,1.,0.));
#9103=DIRECTION('ref_axis',(0.5,0.,-0.866025403784439));
#9104=DIRECTION('center_axis',(0.,1.,0.));
#9105=DIRECTION('ref_axis',(0.5,0.,-0.866025403784438));
#9106=DIRECTION('center_axis',(0.,1.,0.));
#9107=DIRECTION('ref_axis',(0.5,0.,-0.866025403784439));
#9108=DIRECTION('center_axis',(0.,1.,0.));
#9109=DIRECTION('ref_axis',(0.5,0.,-0.866025403784438));
#9110=DIRECTION('center_axis',(0.,1.,0.));
#9111=DIRECTION('ref_axis',(0.5,0.,-0.866025403784439));
#9112=DIRECTION('center_axis',(0.,1.,0.));
#9113=DIRECTION('ref_axis',(0.5,0.,-0.866025403784438));
#9114=DIRECTION('center_axis',(-0.762527203906389,0.,0.646956152534857));
#9115=DIRECTION('ref_axis',(0.646956152534857,0.,0.762527203906389));
#9116=DIRECTION('',(0.646956152534857,0.,0.762527203906389));
#9117=DIRECTION('',(0.,1.,0.));
#9118=DIRECTION('',(0.,1.,0.));
#9119=DIRECTION('center_axis',(-0.695442635009612,0.,0.718581617779698));
#9120=DIRECTION('ref_axis',(0.718581617779698,0.,0.695442635009612));
#9121=DIRECTION('',(0.718581617779698,0.,0.695442635009612));
#9122=DIRECTION('',(0.,1.,0.));
#9123=DIRECTION('center_axis',(-0.621660573370078,0.,0.78328674922865));
#9124=DIRECTION('ref_axis',(0.78328674922865,0.,0.621660573370078));
#9125=DIRECTION('',(0.78328674922865,0.,0.621660573370078));
#9126=DIRECTION('',(0.,1.,0.));
#9127=DIRECTION('center_axis',(-0.541891580574752,0.,0.840448401094438));
#9128=DIRECTION('ref_axis',(0.840448401094438,0.,0.541891580574752));
#9129=DIRECTION('',(0.840448401094438,0.,0.541891580574752));
#9130=DIRECTION('',(0.,1.,0.));
#9131=DIRECTION('center_axis',(-0.456903875630421,0.,0.889516075421856));
#9132=DIRECTION('ref_axis',(0.889516075421856,0.,0.456903875630421));
#9133=DIRECTION('',(0.889516075421856,0.,0.456903875630421));
#9134=DIRECTION('',(0.,1.,0.));
#9135=DIRECTION('center_axis',(-0.367515936594704,0.,0.930017223684012));
#9136=DIRECTION('ref_axis',(0.930017223684012,0.,0.367515936594704));
#9137=DIRECTION('',(0.930017223684012,0.,0.367515936594704));
#9138=DIRECTION('',(0.,1.,0.));
#9139=DIRECTION('center_axis',(-0.274588618184932,0.,0.961561797682962));
#9140=DIRECTION('ref_axis',(0.961561797682962,0.,0.274588618184932));
#9141=DIRECTION('',(0.961561797682962,0.,0.274588618184932));
#9142=DIRECTION('',(0.,1.,0.));
#9143=DIRECTION('center_axis',(-0.179016861276632,0.,0.983846005927078));
#9144=DIRECTION('ref_axis',(0.983846005927078,0.,0.179016861276632));
#9145=DIRECTION('',(0.983846005927077,0.,0.179016861276632));
#9146=DIRECTION('',(0.,1.,0.));
#9147=DIRECTION('center_axis',(-0.99144486137381,0.,-0.130526192220052));
#9148=DIRECTION('ref_axis',(-0.130526192220052,0.,0.99144486137381));
#9149=DIRECTION('',(-0.130526192220052,0.,0.99144486137381));
#9150=DIRECTION('',(0.,1.,0.));
#9151=DIRECTION('center_axis',(0.179016861276632,0.,-0.983846005927078));
#9152=DIRECTION('ref_axis',(-0.983846005927078,0.,-0.179016861276632));
#9153=DIRECTION('',(-0.983846005927078,0.,-0.179016861276632));
#9154=DIRECTION('',(-0.983846005927078,0.,-0.179016861276632));
#9155=DIRECTION('',(0.,1.,0.));
#9156=DIRECTION('center_axis',(0.274588618184932,0.,-0.961561797682962));
#9157=DIRECTION('ref_axis',(-0.961561797682962,0.,-0.274588618184932));
#9158=DIRECTION('',(-0.961561797682962,0.,-0.274588618184932));
#9159=DIRECTION('',(-0.961561797682962,0.,-0.274588618184932));
#9160=DIRECTION('',(0.,1.,0.));
#9161=DIRECTION('center_axis',(0.367515936594703,0.,-0.930017223684013));
#9162=DIRECTION('ref_axis',(-0.930017223684013,0.,-0.367515936594703));
#9163=DIRECTION('',(-0.930017223684013,0.,-0.367515936594703));
#9164=DIRECTION('',(-0.930017223684013,0.,-0.367515936594703));
#9165=DIRECTION('',(0.,1.,0.));
#9166=DIRECTION('center_axis',(0.456903875630423,0.,-0.889516075421855));
#9167=DIRECTION('ref_axis',(-0.889516075421855,0.,-0.456903875630423));
#9168=DIRECTION('',(-0.889516075421855,0.,-0.456903875630423));
#9169=DIRECTION('',(-0.889516075421855,0.,-0.456903875630423));
#9170=DIRECTION('',(0.,1.,0.));
#9171=DIRECTION('center_axis',(0.54189158057475,0.,-0.840448401094439));
#9172=DIRECTION('ref_axis',(-0.840448401094439,0.,-0.54189158057475));
#9173=DIRECTION('',(-0.840448401094439,0.,-0.54189158057475));
#9174=DIRECTION('',(-0.840448401094439,0.,-0.54189158057475));
#9175=DIRECTION('',(0.,1.,0.));
#9176=DIRECTION('center_axis',(0.621660573370078,0.,-0.78328674922865));
#9177=DIRECTION('ref_axis',(-0.78328674922865,0.,-0.621660573370078));
#9178=DIRECTION('',(-0.78328674922865,0.,-0.621660573370078));
#9179=DIRECTION('',(-0.78328674922865,0.,-0.621660573370078));
#9180=DIRECTION('',(0.,1.,0.));
#9181=DIRECTION('center_axis',(0.695442635009612,0.,-0.718581617779698));
#9182=DIRECTION('ref_axis',(-0.718581617779698,0.,-0.695442635009612));
#9183=DIRECTION('',(-0.718581617779698,0.,-0.695442635009612));
#9184=DIRECTION('',(-0.718581617779698,0.,-0.695442635009612));
#9185=DIRECTION('',(0.,1.,0.));
#9186=DIRECTION('center_axis',(0.762527203906389,0.,-0.646956152534857));
#9187=DIRECTION('ref_axis',(-0.646956152534857,0.,-0.762527203906389));
#9188=DIRECTION('',(-0.646956152534857,0.,-0.762527203906389));
#9189=DIRECTION('',(-0.646956152534857,0.,-0.762527203906389));
#9190=DIRECTION('',(0.,1.,0.));
#9191=DIRECTION('center_axis',(0.60876142900872,0.,0.793353340291235));
#9192=DIRECTION('ref_axis',(0.793353340291235,0.,-0.60876142900872));
#9193=DIRECTION('',(0.793353340291235,0.,-0.60876142900872));
#9194=DIRECTION('center_axis',(0.,1.,0.));
#9195=DIRECTION('ref_axis',(0.5,0.,-0.866025403784439));
#9196=DIRECTION('center_axis',(0.,1.,0.));
#9197=DIRECTION('ref_axis',(0.5,0.,-0.866025403784439));
#9198=DIRECTION('center_axis',(0.,1.,0.));
#9199=DIRECTION('ref_axis',(0.5,0.,-0.866025403784438));
#9200=DIRECTION('center_axis',(0.,1.,0.));
#9201=DIRECTION('ref_axis',(0.5,0.,-0.866025403784439));
#9202=DIRECTION('center_axis',(0.,1.,0.));
#9203=DIRECTION('ref_axis',(0.5,0.,-0.866025403784438));
#9204=DIRECTION('center_axis',(0.,1.,0.));
#9205=DIRECTION('ref_axis',(0.5,0.,-0.866025403784439));
#9206=DIRECTION('center_axis',(0.,1.,0.));
#9207=DIRECTION('ref_axis',(0.5,0.,-0.866025403784438));
#9208=DIRECTION('center_axis',(0.,1.,0.));
#9209=DIRECTION('ref_axis',(0.5,0.,-0.866025403784439));
#9210=DIRECTION('center_axis',(0.,1.,0.));
#9211=DIRECTION('ref_axis',(0.5,0.,-0.866025403784438));
#9212=DIRECTION('center_axis',(0.,1.,0.));
#9213=DIRECTION('ref_axis',(0.5,0.,-0.866025403784439));
#9214=DIRECTION('center_axis',(0.,1.,0.));
#9215=DIRECTION('ref_axis',(0.5,0.,-0.866025403784438));
#9216=DIRECTION('center_axis',(0.,1.,0.));
#9217=DIRECTION('ref_axis',(0.5,0.,-0.866025403784439));
#9218=DIRECTION('center_axis',(0.,1.,0.));
#9219=DIRECTION('ref_axis',(0.5,0.,-0.866025403784438));
#9220=DIRECTION('center_axis',(0.,1.,0.));
#9221=DIRECTION('ref_axis',(0.5,0.,-0.866025403784439));
#9222=DIRECTION('center_axis',(0.,1.,0.));
#9223=DIRECTION('ref_axis',(0.5,0.,-0.866025403784438));
#9224=DIRECTION('center_axis',(0.,1.,0.));
#9225=DIRECTION('ref_axis',(0.5,0.,-0.866025403784439));
#9226=DIRECTION('center_axis',(0.,1.,0.));
#9227=DIRECTION('ref_axis',(0.5,0.,-0.866025403784438));
#9228=DIRECTION('center_axis',(0.,1.,0.));
#9229=DIRECTION('ref_axis',(0.5,0.,-0.866025403784438));
#9230=DIRECTION('center_axis',(0.,1.,0.));
#9231=DIRECTION('ref_axis',(0.5,0.,-0.866025403784438));
#9232=DIRECTION('',(0.,-1.,0.));
#9233=DIRECTION('center_axis',(0.,1.,0.));
#9234=DIRECTION('ref_axis',(0.5,0.,-0.866025403784439));
#9235=DIRECTION('axis',(0.,0.,1.));
#9236=DIRECTION('refdir',(1.,0.,0.));
#9237=DIRECTION('center_axis',(0.,1.,0.));
#9238=DIRECTION('ref_axis',(0.866025403784439,0.,-0.5));
#9239=DIRECTION('',(0.121869343405147,0.,0.992546151641322));
#9240=DIRECTION('',(0.994821748296033,0.,-0.101635078182804));
#9241=DIRECTION('',(0.998134798421867,0.,-0.0610485395348574));
#9242=DIRECTION('',(0.999792698085389,0.,-0.0203607675478923));
#9243=DIRECTION('',(0.999792698085388,0.,0.0203607675478936));
#9244=DIRECTION('',(0.998134798421867,0.,0.0610485395348586));
#9245=DIRECTION('',(0.994821748296033,0.,0.101635078182805));
#9246=DIRECTION('',(0.121869343405148,0.,-0.992546151641322));
#9247=DIRECTION('center_axis',(0.,-1.,0.));
#9248=DIRECTION('ref_axis',(0.866025403784439,0.,-0.5));
#9249=DIRECTION('',(-0.798635510047293,0.,0.601815023152048));
#9250=DIRECTION('',(0.585429433769943,0.,0.810723367170211));
#9251=DIRECTION('',(0.551936985312059,0.,0.833885822067168));
#9252=DIRECTION('',(0.517529290979719,0.,0.855665491286186));
#9253=DIRECTION('',(0.482263407105669,0.,0.876026258834079));
#9254=DIRECTION('',(0.446197813109808,0.,0.894934361602026));
#9255=DIRECTION('',(0.40939231452609,0.,0.912358445353015));
#9256=DIRECTION('',(0.92050485345244,0.,-0.390731128489274));
#9257=DIRECTION('center_axis',(0.,-1.,0.));
#9258=DIRECTION('ref_axis',(0.866025403784439,0.,-0.5));
#9259=DIRECTION('',(-0.92050485345244,0.,-0.390731128489274));
#9260=DIRECTION('',(-0.40939231452609,0.,0.912358445353015));
#9261=DIRECTION('',(-0.446197813109808,0.,0.894934361602025));
#9262=DIRECTION('',(-0.482263407105669,0.,0.876026258834078));
#9263=DIRECTION('',(-0.51752929097972,0.,0.855665491286185));
#9264=DIRECTION('',(-0.551936985312059,0.,0.833885822067168));
#9265=DIRECTION('',(-0.585429433769943,0.,0.810723367170211));
#9266=DIRECTION('',(0.798635510047293,0.,0.601815023152048));
#9267=DIRECTION('center_axis',(0.,-1.,0.));
#9268=DIRECTION('ref_axis',(0.866025403784439,0.,-0.5));
#9269=DIRECTION('',(-0.121869343405147,0.,-0.992546151641322));
#9270=DIRECTION('',(-0.994821748296033,0.,0.101635078182804));
#9271=DIRECTION('',(-0.998134798421867,0.,0.0610485395348577));
#9272=DIRECTION('',(-0.999792698085388,0.,0.0203607675478927));
#9273=DIRECTION('',(-0.999792698085389,0.,-0.0203607675478932));
#9274=DIRECTION('',(-0.998134798421867,0.,-0.0610485395348582));
#9275=DIRECTION('',(-0.994821748296033,0.,-0.101635078182805));
#9276=DIRECTION('',(-0.121869343405148,0.,0.992546151641322));
#9277=DIRECTION('center_axis',(0.,-1.,0.));
#9278=DIRECTION('ref_axis',(0.866025403784439,0.,-0.5));
#9279=DIRECTION('',(0.798635510047293,0.,-0.601815023152048));
#9280=DIRECTION('',(-0.585429433769943,0.,-0.810723367170211));
#9281=DIRECTION('',(-0.551936985312059,0.,-0.833885822067168));
#9282=DIRECTION('',(-0.517529290979719,0.,-0.855665491286186));
#9283=DIRECTION('',(-0.482263407105669,0.,-0.876026258834078));
#9284=DIRECTION('',(-0.446197813109808,0.,-0.894934361602026));
#9285=DIRECTION('',(-0.40939231452609,0.,-0.912358445353015));
#9286=DIRECTION('',(-0.92050485345244,0.,0.390731128489274));
#9287=DIRECTION('center_axis',(0.,-1.,0.));
#9288=DIRECTION('ref_axis',(0.866025403784439,0.,-0.5));
#9289=DIRECTION('',(0.92050485345244,0.,0.390731128489275));
#9290=DIRECTION('',(0.409392314526091,0.,-0.912358445353015));
#9291=DIRECTION('',(0.446197813109809,0.,-0.894934361602025));
#9292=DIRECTION('',(0.48226340710567,0.,-0.876026258834078));
#9293=DIRECTION('',(0.51752929097972,0.,-0.855665491286185));
#9294=DIRECTION('',(0.55193698531206,0.,-0.833885822067167));
#9295=DIRECTION('',(0.585429433769943,0.,-0.81072336717021));
#9296=DIRECTION('',(-0.798635510047292,0.,-0.601815023152049));
#9297=DIRECTION('center_axis',(0.,-1.,0.));
#9298=DIRECTION('ref_axis',(0.866025403784439,0.,-0.5));
#9299=DIRECTION('center_axis',(0.,1.,0.));
#9300=DIRECTION('ref_axis',(0.866025403784439,0.,-0.5));
#9301=DIRECTION('',(0.,-1.,0.));
#9302=DIRECTION('center_axis',(0.,1.,0.));
#9303=DIRECTION('ref_axis',(0.866025403784439,0.,-0.5));
#9304=DIRECTION('',(0.,1.,0.));
#9305=DIRECTION('center_axis',(0.,1.,0.));
#9306=DIRECTION('ref_axis',(0.866025403784439,0.,-0.5));
#9307=DIRECTION('',(0.,-1.,0.));
#9308=DIRECTION('center_axis',(0.,1.,0.));
#9309=DIRECTION('ref_axis',(0.866025403784439,0.,-0.5));
#9310=DIRECTION('',(0.,1.,0.));
#9311=DIRECTION('center_axis',(0.,1.,0.));
#9312=DIRECTION('ref_axis',(0.866025403784439,0.,-0.5));
#9313=DIRECTION('',(0.,-1.,0.));
#9314=DIRECTION('center_axis',(0.,1.,0.));
#9315=DIRECTION('ref_axis',(0.866025403784439,0.,-0.5));
#9316=DIRECTION('',(0.,1.,0.));
#9317=DIRECTION('center_axis',(0.,1.,0.));
#9318=DIRECTION('ref_axis',(0.866025403784439,0.,-0.5));
#9319=DIRECTION('',(0.,1.,0.));
#9320=DIRECTION('',(0.,-1.,0.));
#9321=DIRECTION('center_axis',(0.,1.,0.));
#9322=DIRECTION('ref_axis',(0.866025403784439,0.,-0.5));
#9323=DIRECTION('center_axis',(0.,1.,0.));
#9324=DIRECTION('ref_axis',(0.866025403784439,0.,-0.5));
#9325=DIRECTION('',(0.,1.,0.));
#9326=DIRECTION('',(0.,-1.,0.));
#9327=DIRECTION('center_axis',(0.,1.,0.));
#9328=DIRECTION('ref_axis',(0.866025403784439,0.,-0.5));
#9329=DIRECTION('center_axis',(0.,1.,0.));
#9330=DIRECTION('ref_axis',(0.866025403784439,0.,-0.5));
#9331=DIRECTION('',(0.,1.,0.));
#9332=DIRECTION('',(0.,-1.,0.));
#9333=DIRECTION('center_axis',(0.,1.,0.));
#9334=DIRECTION('ref_axis',(0.866025403784439,0.,-0.5));
#9335=DIRECTION('center_axis',(0.,1.,0.));
#9336=DIRECTION('ref_axis',(0.866025403784439,0.,-0.5));
#9337=DIRECTION('',(-0.121869343405147,0.,-0.992546151641322));
#9338=DIRECTION('',(0.798635510047292,0.,0.601815023152049));
#9339=DIRECTION('',(-0.585429433769943,0.,0.81072336717021));
#9340=DIRECTION('',(-0.55193698531206,0.,0.833885822067167));
#9341=DIRECTION('',(-0.51752929097972,0.,0.855665491286185));
#9342=DIRECTION('',(-0.48226340710567,0.,0.876026258834078));
#9343=DIRECTION('',(-0.446197813109809,0.,0.894934361602025));
#9344=DIRECTION('',(-0.409392314526091,0.,0.912358445353015));
#9345=DIRECTION('',(-0.92050485345244,0.,-0.390731128489275));
#9346=DIRECTION('',(0.92050485345244,0.,-0.390731128489274));
#9347=DIRECTION('',(0.40939231452609,0.,0.912358445353015));
#9348=DIRECTION('',(0.446197813109808,0.,0.894934361602026));
#9349=DIRECTION('',(0.482263407105669,0.,0.876026258834078));
#9350=DIRECTION('',(0.517529290979719,0.,0.855665491286186));
#9351=DIRECTION('',(0.551936985312059,0.,0.833885822067168));
#9352=DIRECTION('',(0.585429433769943,0.,0.810723367170211));
#9353=DIRECTION('',(-0.798635510047293,0.,0.601815023152048));
#9354=DIRECTION('',(0.121869343405148,0.,-0.992546151641322));
#9355=DIRECTION('',(0.994821748296033,0.,0.101635078182805));
#9356=DIRECTION('',(0.998134798421867,0.,0.0610485395348582));
#9357=DIRECTION('',(0.999792698085389,0.,0.0203607675478932));
#9358=DIRECTION('',(0.999792698085388,0.,-0.0203607675478927));
#9359=DIRECTION('',(0.998134798421867,0.,-0.0610485395348577));
#9360=DIRECTION('',(0.994821748296033,0.,-0.101635078182804));
#9361=DIRECTION('',(0.121869343405147,0.,0.992546151641322));
#9362=DIRECTION('',(-0.798635510047293,0.,-0.601815023152048));
#9363=DIRECTION('',(0.585429433769943,0.,-0.810723367170211));
#9364=DIRECTION('',(0.551936985312059,0.,-0.833885822067168));
#9365=DIRECTION('',(0.51752929097972,0.,-0.855665491286185));
#9366=DIRECTION('',(0.482263407105669,0.,-0.876026258834078));
#9367=DIRECTION('',(0.446197813109808,0.,-0.894934361602025));
#9368=DIRECTION('',(0.40939231452609,0.,-0.912358445353015));
#9369=DIRECTION('',(0.92050485345244,0.,0.390731128489274));
#9370=DIRECTION('',(-0.92050485345244,0.,0.390731128489274));
#9371=DIRECTION('',(-0.40939231452609,0.,-0.912358445353015));
#9372=DIRECTION('',(-0.446197813109808,0.,-0.894934361602026));
#9373=DIRECTION('',(-0.482263407105669,0.,-0.876026258834079));
#9374=DIRECTION('',(-0.517529290979719,0.,-0.855665491286186));
#9375=DIRECTION('',(-0.551936985312059,0.,-0.833885822067168));
#9376=DIRECTION('',(-0.585429433769943,0.,-0.810723367170211));
#9377=DIRECTION('',(0.798635510047293,0.,-0.601815023152048));
#9378=DIRECTION('',(-0.121869343405148,0.,0.992546151641322));
#9379=DIRECTION('',(-0.994821748296033,0.,-0.101635078182805));
#9380=DIRECTION('',(-0.998134798421867,0.,-0.0610485395348586));
#9381=DIRECTION('',(-0.999792698085388,0.,-0.0203607675478936));
#9382=DIRECTION('',(-0.999792698085389,0.,0.0203607675478923));
#9383=DIRECTION('',(-0.998134798421867,0.,0.0610485395348574));
#9384=DIRECTION('',(-0.994821748296033,0.,0.101635078182804));
#9385=DIRECTION('center_axis',(0.390731128489275,0.,-0.92050485345244));
#9386=DIRECTION('ref_axis',(-0.92050485345244,0.,-0.390731128489275));
#9387=DIRECTION('',(0.,1.,0.));
#9388=DIRECTION('',(-0.92050485345244,0.,-0.390731128489275));
#9389=DIRECTION('',(0.,1.,0.));
#9390=DIRECTION('',(0.92050485345244,0.,0.390731128489275));
#9391=DIRECTION('',(0.,1.,0.));
#9392=DIRECTION('center_axis',(-0.912358445353015,0.,-0.409392314526091));
#9393=DIRECTION('ref_axis',(-0.409392314526091,0.,0.912358445353015));
#9394=DIRECTION('',(0.,1.,0.));
#9395=DIRECTION('',(-0.409392314526091,0.,0.912358445353015));
#9396=DIRECTION('center_axis',(-0.912358445353015,0.,-0.409392314526091));
#9397=DIRECTION('ref_axis',(-0.409392314526091,0.,0.912358445353015));
#9398=DIRECTION('',(0.409392314526091,0.,-0.912358445353015));
#9399=DIRECTION('',(0.,1.,0.));
#9400=DIRECTION('center_axis',(-0.894934361602025,0.,-0.446197813109809));
#9401=DIRECTION('ref_axis',(-0.446197813109809,0.,0.894934361602025));
#9402=DIRECTION('',(0.,1.,0.));
#9403=DIRECTION('',(-0.446197813109809,0.,0.894934361602025));
#9404=DIRECTION('center_axis',(-0.876026258834078,0.,-0.48226340710567));
#9405=DIRECTION('ref_axis',(-0.48226340710567,0.,0.876026258834078));
#9406=DIRECTION('',(0.,1.,0.));
#9407=DIRECTION('',(-0.48226340710567,0.,0.876026258834078));
#9408=DIRECTION('center_axis',(-0.855665491286185,0.,-0.51752929097972));
#9409=DIRECTION('ref_axis',(-0.51752929097972,0.,0.855665491286185));
#9410=DIRECTION('',(0.,1.,0.));
#9411=DIRECTION('',(-0.51752929097972,0.,0.855665491286185));
#9412=DIRECTION('center_axis',(-0.833885822067167,0.,-0.55193698531206));
#9413=DIRECTION('ref_axis',(-0.55193698531206,0.,0.833885822067167));
#9414=DIRECTION('',(0.,1.,0.));
#9415=DIRECTION('',(-0.55193698531206,0.,0.833885822067167));
#9416=DIRECTION('center_axis',(-0.81072336717021,0.,-0.585429433769943));
#9417=DIRECTION('ref_axis',(-0.585429433769943,0.,0.81072336717021));
#9418=DIRECTION('',(0.,-1.,0.));
#9419=DIRECTION('',(-0.585429433769944,0.,0.81072336717021));
#9420=DIRECTION('center_axis',(0.,-1.,0.));
#9421=DIRECTION('ref_axis',(0.500000000000001,0.,-0.866025403784438));
#9422=DIRECTION('',(-0.798635510047292,0.,-0.601815023152049));
#9423=DIRECTION('',(0.585429433769944,0.,-0.81072336717021));
#9424=DIRECTION('',(0.55193698531206,0.,-0.833885822067167));
#9425=DIRECTION('',(0.51752929097972,0.,-0.855665491286185));
#9426=DIRECTION('',(0.48226340710567,0.,-0.876026258834078));
#9427=DIRECTION('',(0.446197813109809,0.,-0.894934361602025));
#9428=DIRECTION('',(-0.409392314526095,0.,0.912358445353013));
#9429=DIRECTION('',(-0.446197813109808,0.,0.894934361602026));
#9430=DIRECTION('',(-0.48226340710567,0.,0.876026258834078));
#9431=DIRECTION('',(-0.51752929097972,0.,0.855665491286185));
#9432=DIRECTION('',(-0.551936985312061,0.,0.833885822067167));
#9433=DIRECTION('',(-0.58542943376994,0.,0.810723367170213));
#9434=DIRECTION('center_axis',(-0.81072336717021,0.,-0.585429433769943));
#9435=DIRECTION('ref_axis',(-0.585429433769943,0.,0.81072336717021));
#9436=DIRECTION('',(0.,1.,0.));
#9437=DIRECTION('',(0.,-1.,0.));
#9438=DIRECTION('center_axis',(-0.833885822067167,0.,-0.55193698531206));
#9439=DIRECTION('ref_axis',(-0.55193698531206,0.,0.833885822067167));
#9440=DIRECTION('',(0.,1.,0.));
#9441=DIRECTION('center_axis',(-0.855665491286185,0.,-0.51752929097972));
#9442=DIRECTION('ref_axis',(-0.51752929097972,0.,0.855665491286185));
#9443=DIRECTION('',(0.,1.,0.));
#9444=DIRECTION('center_axis',(-0.876026258834078,0.,-0.48226340710567));
#9445=DIRECTION('ref_axis',(-0.48226340710567,0.,0.876026258834078));
#9446=DIRECTION('',(0.,1.,0.));
#9447=DIRECTION('center_axis',(-0.894934361602025,0.,-0.446197813109809));
#9448=DIRECTION('ref_axis',(-0.446197813109809,0.,0.894934361602025));
#9449=DIRECTION('center_axis',(0.912358445353013,0.,0.409392314526095));
#9450=DIRECTION('ref_axis',(0.409392314526095,0.,-0.912358445353013));
#9451=DIRECTION('',(0.409392314526095,0.,-0.912358445353013));
#9452=DIRECTION('',(0.,1.,0.));
#9453=DIRECTION('center_axis',(0.894934361602026,0.,0.446197813109808));
#9454=DIRECTION('ref_axis',(0.446197813109808,0.,-0.894934361602026));
#9455=DIRECTION('',(0.446197813109808,0.,-0.894934361602026));
#9456=DIRECTION('',(0.,1.,0.));
#9457=DIRECTION('center_axis',(0.876026258834078,0.,0.48226340710567));
#9458=DIRECTION('ref_axis',(0.48226340710567,0.,-0.876026258834078));
#9459=DIRECTION('',(0.48226340710567,0.,-0.876026258834078));
#9460=DIRECTION('',(0.,1.,0.));
#9461=DIRECTION('center_axis',(0.855665491286185,0.,0.51752929097972));
#9462=DIRECTION('ref_axis',(0.51752929097972,0.,-0.855665491286185));
#9463=DIRECTION('',(0.51752929097972,0.,-0.855665491286185));
#9464=DIRECTION('',(0.,1.,0.));
#9465=DIRECTION('center_axis',(0.833885822067167,0.,0.551936985312061));
#9466=DIRECTION('ref_axis',(0.551936985312061,0.,-0.833885822067167));
#9467=DIRECTION('',(0.551936985312061,0.,-0.833885822067167));
#9468=DIRECTION('',(0.,1.,0.));
#9469=DIRECTION('center_axis',(0.810723367170213,0.,0.58542943376994));
#9470=DIRECTION('ref_axis',(0.58542943376994,0.,-0.810723367170213));
#9471=DIRECTION('',(0.58542943376994,0.,-0.810723367170213));
#9472=DIRECTION('',(0.,1.,0.));
#9473=DIRECTION('center_axis',(-0.601815023152049,0.,0.798635510047292));
#9474=DIRECTION('ref_axis',(0.798635510047292,0.,0.601815023152049));
#9475=DIRECTION('',(0.798635510047292,0.,0.601815023152049));
#9476=DIRECTION('center_axis',(0.,1.,0.));
#9477=DIRECTION('ref_axis',(-0.500000000000001,0.,0.866025403784438));
#9478=DIRECTION('center_axis',(0.601815023152048,0.,0.798635510047293));
#9479=DIRECTION('ref_axis',(0.798635510047293,0.,-0.601815023152048));
#9480=DIRECTION('',(0.,1.,0.));
#9481=DIRECTION('',(0.798635510047293,0.,-0.601815023152048));
#9482=DIRECTION('',(0.,1.,0.));
#9483=DIRECTION('',(-0.798635510047293,0.,0.601815023152048));
#9484=DIRECTION('',(0.,1.,0.));
#9485=DIRECTION('center_axis',(0.810723367170211,0.,-0.585429433769943));
#9486=DIRECTION('ref_axis',(-0.585429433769943,0.,-0.810723367170211));
#9487=DIRECTION('',(0.,1.,0.));
#9488=DIRECTION('',(-0.585429433769943,0.,-0.810723367170211));
#9489=DIRECTION('center_axis',(0.810723367170211,0.,-0.585429433769943));
#9490=DIRECTION('ref_axis',(-0.585429433769943,0.,-0.810723367170211));
#9491=DIRECTION('',(0.585429433769943,0.,0.810723367170211));
#9492=DIRECTION('',(0.,1.,0.));
#9493=DIRECTION('center_axis',(0.833885822067168,0.,-0.551936985312059));
#9494=DIRECTION('ref_axis',(-0.551936985312059,0.,-0.833885822067168));
#9495=DIRECTION('',(0.,1.,0.));
#9496=DIRECTION('',(-0.551936985312059,0.,-0.833885822067168));
#9497=DIRECTION('center_axis',(0.855665491286186,0.,-0.517529290979719));
#9498=DIRECTION('ref_axis',(-0.517529290979719,0.,-0.855665491286186));
#9499=DIRECTION('',(0.,1.,0.));
#9500=DIRECTION('',(-0.517529290979719,0.,-0.855665491286186));
#9501=DIRECTION('center_axis',(0.876026258834078,0.,-0.482263407105669));
#9502=DIRECTION('ref_axis',(-0.482263407105669,0.,-0.876026258834079));
#9503=DIRECTION('',(0.,1.,0.));
#9504=DIRECTION('',(-0.482263407105669,0.,-0.876026258834079));
#9505=DIRECTION('center_axis',(0.894934361602026,0.,-0.446197813109808));
#9506=DIRECTION('ref_axis',(-0.446197813109808,0.,-0.894934361602026));
#9507=DIRECTION('',(0.,1.,0.));
#9508=DIRECTION('',(-0.446197813109808,0.,-0.894934361602026));
#9509=DIRECTION('center_axis',(0.912358445353015,0.,-0.40939231452609));
#9510=DIRECTION('ref_axis',(-0.40939231452609,0.,-0.912358445353015));
#9511=DIRECTION('',(0.,-1.,0.));
#9512=DIRECTION('',(-0.40939231452609,0.,-0.912358445353015));
#9513=DIRECTION('center_axis',(0.,-1.,0.));
#9514=DIRECTION('ref_axis',(0.5,0.,0.866025403784439));
#9515=DIRECTION('',(0.92050485345244,0.,-0.390731128489274));
#9516=DIRECTION('',(0.40939231452609,0.,0.912358445353015));
#9517=DIRECTION('',(0.446197813109808,0.,0.894934361602026));
#9518=DIRECTION('',(0.482263407105669,0.,0.876026258834079));
#9519=DIRECTION('',(0.517529290979719,0.,0.855665491286186));
#9520=DIRECTION('',(0.551936985312059,0.,0.833885822067168));
#9521=DIRECTION('',(-0.585429433769939,0.,-0.810723367170213));
#9522=DIRECTION('',(-0.55193698531206,0.,-0.833885822067167));
#9523=DIRECTION('',(-0.517529290979719,0.,-0.855665491286186));
#9524=DIRECTION('',(-0.482263407105669,0.,-0.876026258834078));
#9525=DIRECTION('',(-0.446197813109807,0.,-0.894934361602026));
#9526=DIRECTION('',(-0.409392314526094,0.,-0.912358445353014));
#9527=DIRECTION('center_axis',(0.912358445353015,0.,-0.40939231452609));
#9528=DIRECTION('ref_axis',(-0.40939231452609,0.,-0.912358445353015));
#9529=DIRECTION('',(0.,1.,0.));
#9530=DIRECTION('',(0.,-1.,0.));
#9531=DIRECTION('center_axis',(0.894934361602026,0.,-0.446197813109808));
#9532=DIRECTION('ref_axis',(-0.446197813109808,0.,-0.894934361602026));
#9533=DIRECTION('',(0.,1.,0.));
#9534=DIRECTION('center_axis',(0.876026258834078,0.,-0.482263407105669));
#9535=DIRECTION('ref_axis',(-0.482263407105669,0.,-0.876026258834079));
#9536=DIRECTION('',(0.,1.,0.));
#9537=DIRECTION('center_axis',(0.855665491286186,0.,-0.517529290979719));
#9538=DIRECTION('ref_axis',(-0.517529290979719,0.,-0.855665491286186));
#9539=DIRECTION('',(0.,1.,0.));
#9540=DIRECTION('center_axis',(0.833885822067168,0.,-0.551936985312059));
#9541=DIRECTION('ref_axis',(-0.551936985312059,0.,-0.833885822067168));
#9542=DIRECTION('center_axis',(-0.810723367170213,0.,0.585429433769939));
#9543=DIRECTION('ref_axis',(0.585429433769939,0.,0.810723367170213));
#9544=DIRECTION('',(0.585429433769939,0.,0.810723367170213));
#9545=DIRECTION('',(0.,1.,0.));
#9546=DIRECTION('center_axis',(-0.833885822067167,0.,0.55193698531206));
#9547=DIRECTION('ref_axis',(0.55193698531206,0.,0.833885822067167));
#9548=DIRECTION('',(0.55193698531206,0.,0.833885822067167));
#9549=DIRECTION('',(0.,1.,0.));
#9550=DIRECTION('center_axis',(-0.855665491286186,0.,0.517529290979719));
#9551=DIRECTION('ref_axis',(0.517529290979719,0.,0.855665491286186));
#9552=DIRECTION('',(0.517529290979719,0.,0.855665491286186));
#9553=DIRECTION('',(0.,1.,0.));
#9554=DIRECTION('center_axis',(-0.876026258834078,0.,0.482263407105669));
#9555=DIRECTION('ref_axis',(0.482263407105669,0.,0.876026258834078));
#9556=DIRECTION('',(0.482263407105669,0.,0.876026258834078));
#9557=DIRECTION('',(0.,1.,0.));
#9558=DIRECTION('center_axis',(-0.894934361602026,0.,0.446197813109807));
#9559=DIRECTION('ref_axis',(0.446197813109807,0.,0.894934361602026));
#9560=DIRECTION('',(0.446197813109807,0.,0.894934361602026));
#9561=DIRECTION('',(0.,1.,0.));
#9562=DIRECTION('center_axis',(-0.912358445353014,0.,0.409392314526094));
#9563=DIRECTION('ref_axis',(0.409392314526094,0.,0.912358445353014));
#9564=DIRECTION('',(0.409392314526094,0.,0.912358445353014));
#9565=DIRECTION('',(0.,1.,0.));
#9566=DIRECTION('center_axis',(-0.390731128489274,0.,-0.92050485345244));
#9567=DIRECTION('ref_axis',(-0.92050485345244,0.,0.390731128489274));
#9568=DIRECTION('',(-0.92050485345244,0.,0.390731128489274));
#9569=DIRECTION('center_axis',(0.,1.,0.));
#9570=DIRECTION('ref_axis',(-0.5,0.,-0.866025403784439));
#9571=DIRECTION('center_axis',(-0.992546151641322,0.,0.121869343405147));
#9572=DIRECTION('ref_axis',(0.121869343405147,0.,0.992546151641322));
#9573=DIRECTION('',(0.,1.,0.));
#9574=DIRECTION('',(0.121869343405147,0.,0.992546151641322));
#9575=DIRECTION('',(0.,1.,0.));
#9576=DIRECTION('',(-0.121869343405147,0.,-0.992546151641322));
#9577=DIRECTION('',(0.,1.,0.));
#9578=DIRECTION('center_axis',(0.101635078182804,0.,0.994821748296033));
#9579=DIRECTION('ref_axis',(0.994821748296033,0.,-0.101635078182804));
#9580=DIRECTION('',(0.,1.,0.));
#9581=DIRECTION('',(0.994821748296033,0.,-0.101635078182804));
#9582=DIRECTION('center_axis',(0.101635078182804,0.,0.994821748296033));
#9583=DIRECTION('ref_axis',(0.994821748296033,0.,-0.101635078182804));
#9584=DIRECTION('',(-0.994821748296033,0.,0.101635078182804));
#9585=DIRECTION('',(0.,1.,0.));
#9586=DIRECTION('center_axis',(0.0610485395348577,0.,0.998134798421867));
#9587=DIRECTION('ref_axis',(0.998134798421867,0.,-0.0610485395348577));
#9588=DIRECTION('',(0.,1.,0.));
#9589=DIRECTION('',(0.998134798421867,0.,-0.0610485395348577));
#9590=DIRECTION('center_axis',(0.0203607675478927,0.,0.999792698085389));
#9591=DIRECTION('ref_axis',(0.999792698085388,0.,-0.0203607675478927));
#9592=DIRECTION('',(0.,1.,0.));
#9593=DIRECTION('',(0.999792698085388,0.,-0.0203607675478927));
#9594=DIRECTION('center_axis',(-0.0203607675478932,0.,0.999792698085389));
#9595=DIRECTION('ref_axis',(0.999792698085389,0.,0.0203607675478932));
#9596=DIRECTION('',(0.,1.,0.));
#9597=DIRECTION('',(0.999792698085389,0.,0.0203607675478932));
#9598=DIRECTION('center_axis',(-0.0610485395348582,0.,0.998134798421867));
#9599=DIRECTION('ref_axis',(0.998134798421867,0.,0.0610485395348582));
#9600=DIRECTION('',(0.,1.,0.));
#9601=DIRECTION('',(0.998134798421867,0.,0.0610485395348582));
#9602=DIRECTION('center_axis',(-0.101635078182805,0.,0.994821748296033));
#9603=DIRECTION('ref_axis',(0.994821748296033,0.,0.101635078182805));
#9604=DIRECTION('',(0.,-1.,0.));
#9605=DIRECTION('',(0.994821748296033,0.,0.101635078182805));
#9606=DIRECTION('center_axis',(0.,-1.,0.));
#9607=DIRECTION('ref_axis',(-1.,0.,-2.22044604925031E-16));
#9608=DIRECTION('',(-0.121869343405148,0.,0.992546151641322));
#9609=DIRECTION('',(-0.994821748296033,0.,-0.101635078182805));
#9610=DIRECTION('',(-0.998134798421867,0.,-0.0610485395348582));
#9611=DIRECTION('',(-0.999792698085389,0.,-0.0203607675478932));
#9612=DIRECTION('',(-0.999792698085388,0.,0.0203607675478927));
#9613=DIRECTION('',(-0.998134798421867,0.,0.0610485395348577));
#9614=DIRECTION('',(0.994821748296033,0.,-0.1016350781828));
#9615=DIRECTION('',(0.998134798421867,0.,-0.0610485395348589));
#9616=DIRECTION('',(0.999792698085388,0.,-0.0203607675478925));
#9617=DIRECTION('',(0.999792698085389,0.,0.0203607675478929));
#9618=DIRECTION('',(0.998134798421867,0.,0.0610485395348593));
#9619=DIRECTION('',(0.994821748296033,0.,0.1016350781828));
#9620=DIRECTION('center_axis',(-0.101635078182805,0.,0.994821748296033));
#9621=DIRECTION('ref_axis',(0.994821748296033,0.,0.101635078182805));
#9622=DIRECTION('',(0.,1.,0.));
#9623=DIRECTION('',(0.,-1.,0.));
#9624=DIRECTION('center_axis',(-0.0610485395348582,0.,0.998134798421867));
#9625=DIRECTION('ref_axis',(0.998134798421867,0.,0.0610485395348582));
#9626=DIRECTION('',(0.,1.,0.));
#9627=DIRECTION('center_axis',(-0.0203607675478932,0.,0.999792698085389));
#9628=DIRECTION('ref_axis',(0.999792698085389,0.,0.0203607675478932));
#9629=DIRECTION('',(0.,1.,0.));
#9630=DIRECTION('center_axis',(0.0203607675478927,0.,0.999792698085389));
#9631=DIRECTION('ref_axis',(0.999792698085388,0.,-0.0203607675478927));
#9632=DIRECTION('',(0.,1.,0.));
#9633=DIRECTION('center_axis',(0.0610485395348577,0.,0.998134798421867));
#9634=DIRECTION('ref_axis',(0.998134798421867,0.,-0.0610485395348577));
#9635=DIRECTION('center_axis',(-0.1016350781828,0.,-0.994821748296033));
#9636=DIRECTION('ref_axis',(-0.994821748296033,0.,0.1016350781828));
#9637=DIRECTION('',(-0.994821748296033,0.,0.1016350781828));
#9638=DIRECTION('',(0.,1.,0.));
#9639=DIRECTION('center_axis',(-0.0610485395348589,0.,-0.998134798421867));
#9640=DIRECTION('ref_axis',(-0.998134798421867,0.,0.0610485395348589));
#9641=DIRECTION('',(-0.998134798421867,0.,0.0610485395348589));
#9642=DIRECTION('',(0.,1.,0.));
#9643=DIRECTION('center_axis',(-0.0203607675478925,0.,-0.999792698085389));
#9644=DIRECTION('ref_axis',(-0.999792698085388,0.,0.0203607675478925));
#9645=DIRECTION('',(-0.999792698085388,0.,0.0203607675478925));
#9646=DIRECTION('',(0.,1.,0.));
#9647=DIRECTION('center_axis',(0.0203607675478929,0.,-0.999792698085389));
#9648=DIRECTION('ref_axis',(-0.999792698085389,0.,-0.0203607675478929));
#9649=DIRECTION('',(-0.999792698085389,0.,-0.0203607675478929));
#9650=DIRECTION('',(0.,1.,0.));
#9651=DIRECTION('center_axis',(0.0610485395348593,0.,-0.998134798421867));
#9652=DIRECTION('ref_axis',(-0.998134798421867,0.,-0.0610485395348593));
#9653=DIRECTION('',(-0.998134798421867,0.,-0.0610485395348593));
#9654=DIRECTION('',(0.,1.,0.));
#9655=DIRECTION('center_axis',(0.1016350781828,0.,-0.994821748296033));
#9656=DIRECTION('ref_axis',(-0.994821748296033,0.,-0.1016350781828));
#9657=DIRECTION('',(-0.994821748296033,0.,-0.1016350781828));
#9658=DIRECTION('',(0.,1.,0.));
#9659=DIRECTION('center_axis',(0.992546151641322,0.,0.121869343405148));
#9660=DIRECTION('ref_axis',(0.121869343405148,0.,-0.992546151641322));
#9661=DIRECTION('',(0.121869343405148,0.,-0.992546151641322));
#9662=DIRECTION('center_axis',(0.,1.,0.));
#9663=DIRECTION('ref_axis',(1.,0.,2.22044604925031E-16));
#9664=DIRECTION('center_axis',(-0.601815023152048,0.,-0.798635510047293));
#9665=DIRECTION('ref_axis',(-0.798635510047293,0.,0.601815023152048));
#9666=DIRECTION('',(0.,1.,0.));
#9667=DIRECTION('',(-0.798635510047293,0.,0.601815023152048));
#9668=DIRECTION('',(0.,1.,0.));
#9669=DIRECTION('',(0.798635510047293,0.,-0.601815023152048));
#9670=DIRECTION('',(0.,1.,0.));
#9671=DIRECTION('center_axis',(-0.810723367170211,0.,0.585429433769943));
#9672=DIRECTION('ref_axis',(0.585429433769943,0.,0.810723367170211));
#9673=DIRECTION('',(0.,1.,0.));
#9674=DIRECTION('',(0.585429433769943,0.,0.810723367170211));
#9675=DIRECTION('center_axis',(-0.810723367170211,0.,0.585429433769943));
#9676=DIRECTION('ref_axis',(0.585429433769943,0.,0.810723367170211));
#9677=DIRECTION('',(-0.585429433769943,0.,-0.810723367170211));
#9678=DIRECTION('',(0.,1.,0.));
#9679=DIRECTION('center_axis',(-0.833885822067168,0.,0.551936985312059));
#9680=DIRECTION('ref_axis',(0.551936985312059,0.,0.833885822067168));
#9681=DIRECTION('',(0.,1.,0.));
#9682=DIRECTION('',(0.551936985312059,0.,0.833885822067168));
#9683=DIRECTION('center_axis',(-0.855665491286186,0.,0.517529290979719));
#9684=DIRECTION('ref_axis',(0.517529290979719,0.,0.855665491286186));
#9685=DIRECTION('',(0.,1.,0.));
#9686=DIRECTION('',(0.517529290979719,0.,0.855665491286186));
#9687=DIRECTION('center_axis',(-0.876026258834078,0.,0.482263407105669));
#9688=DIRECTION('ref_axis',(0.482263407105669,0.,0.876026258834078));
#9689=DIRECTION('',(0.,1.,0.));
#9690=DIRECTION('',(0.482263407105669,0.,0.876026258834078));
#9691=DIRECTION('center_axis',(-0.894934361602026,0.,0.446197813109808));
#9692=DIRECTION('ref_axis',(0.446197813109808,0.,0.894934361602026));
#9693=DIRECTION('',(0.,1.,0.));
#9694=DIRECTION('',(0.446197813109808,0.,0.894934361602026));
#9695=DIRECTION('center_axis',(-0.912358445353015,0.,0.40939231452609));
#9696=DIRECTION('ref_axis',(0.40939231452609,0.,0.912358445353015));
#9697=DIRECTION('',(0.,-1.,0.));
#9698=DIRECTION('',(0.40939231452609,0.,0.912358445353015));
#9699=DIRECTION('center_axis',(0.,-1.,0.));
#9700=DIRECTION('ref_axis',(-0.5,0.,-0.866025403784439));
#9701=DIRECTION('',(-0.92050485345244,0.,0.390731128489274));
#9702=DIRECTION('',(-0.40939231452609,0.,-0.912358445353015));
#9703=DIRECTION('',(-0.446197813109808,0.,-0.894934361602026));
#9704=DIRECTION('',(-0.482263407105669,0.,-0.876026258834078));
#9705=DIRECTION('',(-0.517529290979719,0.,-0.855665491286186));
#9706=DIRECTION('',(-0.551936985312059,0.,-0.833885822067168));
#9707=DIRECTION('',(0.585429433769939,0.,0.810723367170213));
#9708=DIRECTION('',(0.55193698531206,0.,0.833885822067167));
#9709=DIRECTION('',(0.517529290979719,0.,0.855665491286186));
#9710=DIRECTION('',(0.482263407105669,0.,0.876026258834078));
#9711=DIRECTION('',(0.446197813109807,0.,0.894934361602026));
#9712=DIRECTION('',(0.409392314526094,0.,0.912358445353014));
#9713=DIRECTION('center_axis',(-0.912358445353015,0.,0.40939231452609));
#9714=DIRECTION('ref_axis',(0.40939231452609,0.,0.912358445353015));
#9715=DIRECTION('',(0.,1.,0.));
#9716=DIRECTION('',(0.,-1.,0.));
#9717=DIRECTION('center_axis',(-0.894934361602026,0.,0.446197813109808));
#9718=DIRECTION('ref_axis',(0.446197813109808,0.,0.894934361602026));
#9719=DIRECTION('',(0.,1.,0.));
#9720=DIRECTION('center_axis',(-0.876026258834078,0.,0.482263407105669));
#9721=DIRECTION('ref_axis',(0.482263407105669,0.,0.876026258834078));
#9722=DIRECTION('',(0.,1.,0.));
#9723=DIRECTION('center_axis',(-0.855665491286186,0.,0.517529290979719));
#9724=DIRECTION('ref_axis',(0.517529290979719,0.,0.855665491286186));
#9725=DIRECTION('',(0.,1.,0.));
#9726=DIRECTION('center_axis',(-0.833885822067168,0.,0.551936985312059));
#9727=DIRECTION('ref_axis',(0.551936985312059,0.,0.833885822067168));
#9728=DIRECTION('center_axis',(0.810723367170213,0.,-0.585429433769939));
#9729=DIRECTION('ref_axis',(-0.585429433769939,0.,-0.810723367170213));
#9730=DIRECTION('',(-0.585429433769939,0.,-0.810723367170213));
#9731=DIRECTION('',(0.,1.,0.));
#9732=DIRECTION('center_axis',(0.833885822067167,0.,-0.55193698531206));
#9733=DIRECTION('ref_axis',(-0.55193698531206,0.,-0.833885822067167));
#9734=DIRECTION('',(-0.55193698531206,0.,-0.833885822067167));
#9735=DIRECTION('',(0.,1.,0.));
#9736=DIRECTION('center_axis',(0.855665491286186,0.,-0.517529290979719));
#9737=DIRECTION('ref_axis',(-0.517529290979719,0.,-0.855665491286186));
#9738=DIRECTION('',(-0.517529290979719,0.,-0.855665491286186));
#9739=DIRECTION('',(0.,1.,0.));
#9740=DIRECTION('center_axis',(0.876026258834078,0.,-0.482263407105669));
#9741=DIRECTION('ref_axis',(-0.482263407105669,0.,-0.876026258834078));
#9742=DIRECTION('',(-0.482263407105669,0.,-0.876026258834078));
#9743=DIRECTION('',(0.,1.,0.));
#9744=DIRECTION('center_axis',(0.894934361602026,0.,-0.446197813109807));
#9745=DIRECTION('ref_axis',(-0.446197813109807,0.,-0.894934361602026));
#9746=DIRECTION('',(-0.446197813109807,0.,-0.894934361602026));
#9747=DIRECTION('',(0.,1.,0.));
#9748=DIRECTION('center_axis',(0.912358445353014,0.,-0.409392314526094));
#9749=DIRECTION('ref_axis',(-0.409392314526094,0.,-0.912358445353014));
#9750=DIRECTION('',(-0.409392314526094,0.,-0.912358445353014));
#9751=DIRECTION('',(0.,1.,0.));
#9752=DIRECTION('center_axis',(0.390731128489274,0.,0.92050485345244));
#9753=DIRECTION('ref_axis',(0.92050485345244,0.,-0.390731128489274));
#9754=DIRECTION('',(0.92050485345244,0.,-0.390731128489274));
#9755=DIRECTION('center_axis',(0.,1.,0.));
#9756=DIRECTION('ref_axis',(0.5,0.,0.866025403784439));
#9757=DIRECTION('center_axis',(-0.390731128489274,0.,0.92050485345244));
#9758=DIRECTION('ref_axis',(0.92050485345244,0.,0.390731128489274));
#9759=DIRECTION('',(0.,1.,0.));
#9760=DIRECTION('',(0.92050485345244,0.,0.390731128489274));
#9761=DIRECTION('',(0.,1.,0.));
#9762=DIRECTION('',(-0.92050485345244,0.,-0.390731128489274));
#9763=DIRECTION('',(0.,1.,0.));
#9764=DIRECTION('center_axis',(0.912358445353015,0.,0.40939231452609));
#9765=DIRECTION('ref_axis',(0.40939231452609,0.,-0.912358445353015));
#9766=DIRECTION('',(0.,1.,0.));
#9767=DIRECTION('',(0.40939231452609,0.,-0.912358445353015));
#9768=DIRECTION('center_axis',(0.912358445353015,0.,0.40939231452609));
#9769=DIRECTION('ref_axis',(0.40939231452609,0.,-0.912358445353015));
#9770=DIRECTION('',(-0.40939231452609,0.,0.912358445353015));
#9771=DIRECTION('',(0.,1.,0.));
#9772=DIRECTION('center_axis',(0.894934361602025,0.,0.446197813109808));
#9773=DIRECTION('ref_axis',(0.446197813109808,0.,-0.894934361602025));
#9774=DIRECTION('',(0.,1.,0.));
#9775=DIRECTION('',(0.446197813109808,0.,-0.894934361602025));
#9776=DIRECTION('center_axis',(0.876026258834078,0.,0.482263407105669));
#9777=DIRECTION('ref_axis',(0.482263407105669,0.,-0.876026258834078));
#9778=DIRECTION('',(0.,1.,0.));
#9779=DIRECTION('',(0.482263407105669,0.,-0.876026258834078));
#9780=DIRECTION('center_axis',(0.855665491286185,0.,0.51752929097972));
#9781=DIRECTION('ref_axis',(0.51752929097972,0.,-0.855665491286185));
#9782=DIRECTION('',(0.,1.,0.));
#9783=DIRECTION('',(0.51752929097972,0.,-0.855665491286185));
#9784=DIRECTION('center_axis',(0.833885822067168,0.,0.551936985312059));
#9785=DIRECTION('ref_axis',(0.551936985312059,0.,-0.833885822067168));
#9786=DIRECTION('',(0.,1.,0.));
#9787=DIRECTION('',(0.551936985312059,0.,-0.833885822067167));
#9788=DIRECTION('center_axis',(0.810723367170211,0.,0.585429433769943));
#9789=DIRECTION('ref_axis',(0.585429433769943,0.,-0.810723367170211));
#9790=DIRECTION('',(0.,-1.,0.));
#9791=DIRECTION('',(0.585429433769943,0.,-0.810723367170211));
#9792=DIRECTION('center_axis',(0.,-1.,0.));
#9793=DIRECTION('ref_axis',(-0.5,0.,0.866025403784439));
#9794=DIRECTION('',(0.798635510047293,0.,0.601815023152048));
#9795=DIRECTION('',(-0.585429433769943,0.,0.810723367170211));
#9796=DIRECTION('',(-0.551936985312059,0.,0.833885822067167));
#9797=DIRECTION('',(-0.51752929097972,0.,0.855665491286185));
#9798=DIRECTION('',(-0.482263407105669,0.,0.876026258834078));
#9799=DIRECTION('',(-0.446197813109808,0.,0.894934361602025));
#9800=DIRECTION('',(0.409392314526094,0.,-0.912358445353013));
#9801=DIRECTION('',(0.446197813109807,0.,-0.894934361602026));
#9802=DIRECTION('',(0.48226340710567,0.,-0.876026258834078));
#9803=DIRECTION('',(0.517529290979719,0.,-0.855665491286185));
#9804=DIRECTION('',(0.55193698531206,0.,-0.833885822067167));
#9805=DIRECTION('',(0.58542943376994,0.,-0.810723367170213));
#9806=DIRECTION('center_axis',(0.810723367170211,0.,0.585429433769943));
#9807=DIRECTION('ref_axis',(0.585429433769943,0.,-0.810723367170211));
#9808=DIRECTION('',(0.,1.,0.));
#9809=DIRECTION('',(0.,-1.,0.));
#9810=DIRECTION('center_axis',(0.833885822067168,0.,0.551936985312059));
#9811=DIRECTION('ref_axis',(0.551936985312059,0.,-0.833885822067168));
#9812=DIRECTION('',(0.,1.,0.));
#9813=DIRECTION('center_axis',(0.855665491286185,0.,0.51752929097972));
#9814=DIRECTION('ref_axis',(0.51752929097972,0.,-0.855665491286185));
#9815=DIRECTION('',(0.,1.,0.));
#9816=DIRECTION('center_axis',(0.876026258834078,0.,0.482263407105669));
#9817=DIRECTION('ref_axis',(0.482263407105669,0.,-0.876026258834078));
#9818=DIRECTION('',(0.,1.,0.));
#9819=DIRECTION('center_axis',(0.894934361602025,0.,0.446197813109808));
#9820=DIRECTION('ref_axis',(0.446197813109808,0.,-0.894934361602025));
#9821=DIRECTION('center_axis',(-0.912358445353013,0.,-0.409392314526094));
#9822=DIRECTION('ref_axis',(-0.409392314526094,0.,0.912358445353013));
#9823=DIRECTION('',(-0.409392314526094,0.,0.912358445353013));
#9824=DIRECTION('',(0.,1.,0.));
#9825=DIRECTION('center_axis',(-0.894934361602026,0.,-0.446197813109807));
#9826=DIRECTION('ref_axis',(-0.446197813109807,0.,0.894934361602026));
#9827=DIRECTION('',(-0.446197813109807,0.,0.894934361602026));
#9828=DIRECTION('',(0.,1.,0.));
#9829=DIRECTION('center_axis',(-0.876026258834078,0.,-0.48226340710567));
#9830=DIRECTION('ref_axis',(-0.48226340710567,0.,0.876026258834078));
#9831=DIRECTION('',(-0.48226340710567,0.,0.876026258834078));
#9832=DIRECTION('',(0.,1.,0.));
#9833=DIRECTION('center_axis',(-0.855665491286185,0.,-0.517529290979719));
#9834=DIRECTION('ref_axis',(-0.517529290979719,0.,0.855665491286185));
#9835=DIRECTION('',(-0.517529290979719,0.,0.855665491286185));
#9836=DIRECTION('',(0.,1.,0.));
#9837=DIRECTION('center_axis',(-0.833885822067167,0.,-0.55193698531206));
#9838=DIRECTION('ref_axis',(-0.55193698531206,0.,0.833885822067167));
#9839=DIRECTION('',(-0.55193698531206,0.,0.833885822067167));
#9840=DIRECTION('',(0.,1.,0.));
#9841=DIRECTION('center_axis',(-0.810723367170213,0.,-0.585429433769939));
#9842=DIRECTION('ref_axis',(-0.585429433769939,0.,0.810723367170213));
#9843=DIRECTION('',(-0.58542943376994,0.,0.810723367170213));
#9844=DIRECTION('',(0.,1.,0.));
#9845=DIRECTION('center_axis',(0.601815023152048,0.,-0.798635510047293));
#9846=DIRECTION('ref_axis',(-0.798635510047293,0.,-0.601815023152048));
#9847=DIRECTION('',(-0.798635510047293,0.,-0.601815023152048));
#9848=DIRECTION('center_axis',(0.,1.,0.));
#9849=DIRECTION('ref_axis',(0.5,0.,-0.866025403784439));
#9850=DIRECTION('center_axis',(0.992546151641322,0.,-0.121869343405147));
#9851=DIRECTION('ref_axis',(-0.121869343405147,0.,-0.992546151641322));
#9852=DIRECTION('',(0.,1.,0.));
#9853=DIRECTION('',(-0.121869343405147,0.,-0.992546151641322));
#9854=DIRECTION('',(0.,1.,0.));
#9855=DIRECTION('',(0.121869343405147,0.,0.992546151641322));
#9856=DIRECTION('',(0.,1.,0.));
#9857=DIRECTION('center_axis',(-0.101635078182804,0.,-0.994821748296033));
#9858=DIRECTION('ref_axis',(-0.994821748296033,0.,0.101635078182804));
#9859=DIRECTION('',(0.,1.,0.));
#9860=DIRECTION('',(-0.994821748296033,0.,0.101635078182804));
#9861=DIRECTION('center_axis',(-0.101635078182804,0.,-0.994821748296033));
#9862=DIRECTION('ref_axis',(-0.994821748296033,0.,0.101635078182804));
#9863=DIRECTION('',(0.994821748296033,0.,-0.101635078182804));
#9864=DIRECTION('',(0.,1.,0.));
#9865=DIRECTION('center_axis',(-0.0610485395348574,0.,-0.998134798421867));
#9866=DIRECTION('ref_axis',(-0.998134798421867,0.,0.0610485395348574));
#9867=DIRECTION('',(0.,1.,0.));
#9868=DIRECTION('',(-0.998134798421867,0.,0.0610485395348574));
#9869=DIRECTION('center_axis',(-0.0203607675478923,0.,-0.999792698085389));
#9870=DIRECTION('ref_axis',(-0.999792698085389,0.,0.0203607675478923));
#9871=DIRECTION('',(0.,1.,0.));
#9872=DIRECTION('',(-0.999792698085389,0.,0.0203607675478923));
#9873=DIRECTION('center_axis',(0.0203607675478936,0.,-0.999792698085388));
#9874=DIRECTION('ref_axis',(-0.999792698085388,0.,-0.0203607675478936));
#9875=DIRECTION('',(0.,1.,0.));
#9876=DIRECTION('',(-0.999792698085388,0.,-0.0203607675478936));
#9877=DIRECTION('center_axis',(0.0610485395348586,0.,-0.998134798421867));
#9878=DIRECTION('ref_axis',(-0.998134798421867,0.,-0.0610485395348586));
#9879=DIRECTION('',(0.,1.,0.));
#9880=DIRECTION('',(-0.998134798421867,0.,-0.0610485395348586));
#9881=DIRECTION('center_axis',(0.101635078182805,0.,-0.994821748296033));
#9882=DIRECTION('ref_axis',(-0.994821748296033,0.,-0.101635078182805));
#9883=DIRECTION('',(0.,-1.,0.));
#9884=DIRECTION('',(-0.994821748296033,0.,-0.101635078182805));
#9885=DIRECTION('center_axis',(0.,-1.,0.));
#9886=DIRECTION('ref_axis',(1.,0.,6.10622663543836E-16));
#9887=DIRECTION('',(0.121869343405148,0.,-0.992546151641322));
#9888=DIRECTION('',(0.994821748296033,0.,0.101635078182805));
#9889=DIRECTION('',(0.998134798421867,0.,0.0610485395348586));
#9890=DIRECTION('',(0.999792698085388,0.,0.0203607675478936));
#9891=DIRECTION('',(0.999792698085389,0.,-0.0203607675478923));
#9892=DIRECTION('',(0.998134798421867,0.,-0.0610485395348574));
#9893=DIRECTION('',(-0.994821748296033,0.,0.1016350781828));
#9894=DIRECTION('',(-0.998134798421867,0.,0.0610485395348585));
#9895=DIRECTION('',(-0.999792698085389,0.,0.0203607675478921));
#9896=DIRECTION('',(-0.999792698085388,0.,-0.0203607675478933));
#9897=DIRECTION('',(-0.998134798421867,0.,-0.0610485395348597));
#9898=DIRECTION('',(-0.994821748296033,0.,-0.101635078182801));
#9899=DIRECTION('center_axis',(0.101635078182805,0.,-0.994821748296033));
#9900=DIRECTION('ref_axis',(-0.994821748296033,0.,-0.101635078182805));
#9901=DIRECTION('',(0.,1.,0.));
#9902=DIRECTION('',(0.,-1.,0.));
#9903=DIRECTION('center_axis',(0.0610485395348586,0.,-0.998134798421867));
#9904=DIRECTION('ref_axis',(-0.998134798421867,0.,-0.0610485395348586));
#9905=DIRECTION('',(0.,1.,0.));
#9906=DIRECTION('center_axis',(0.0203607675478936,0.,-0.999792698085388));
#9907=DIRECTION('ref_axis',(-0.999792698085388,0.,-0.0203607675478936));
#9908=DIRECTION('',(0.,1.,0.));
#9909=DIRECTION('center_axis',(-0.0203607675478923,0.,-0.999792698085389));
#9910=DIRECTION('ref_axis',(-0.999792698085389,0.,0.0203607675478923));
#9911=DIRECTION('',(0.,1.,0.));
#9912=DIRECTION('center_axis',(-0.0610485395348574,0.,-0.998134798421867));
#9913=DIRECTION('ref_axis',(-0.998134798421867,0.,0.0610485395348574));
#9914=DIRECTION('center_axis',(0.1016350781828,0.,0.994821748296033));
#9915=DIRECTION('ref_axis',(0.994821748296033,0.,-0.1016350781828));
#9916=DIRECTION('',(0.994821748296033,0.,-0.1016350781828));
#9917=DIRECTION('',(0.,1.,0.));
#9918=DIRECTION('center_axis',(0.0610485395348585,0.,0.998134798421867));
#9919=DIRECTION('ref_axis',(0.998134798421867,0.,-0.0610485395348585));
#9920=DIRECTION('',(0.998134798421867,0.,-0.0610485395348585));
#9921=DIRECTION('',(0.,1.,0.));
#9922=DIRECTION('center_axis',(0.0203607675478921,0.,0.999792698085389));
#9923=DIRECTION('ref_axis',(0.999792698085389,0.,-0.0203607675478921));
#9924=DIRECTION('',(0.999792698085389,0.,-0.0203607675478921));
#9925=DIRECTION('',(0.,1.,0.));
#9926=DIRECTION('center_axis',(-0.0203607675478933,0.,0.999792698085389));
#9927=DIRECTION('ref_axis',(0.999792698085388,0.,0.0203607675478933));
#9928=DIRECTION('',(0.999792698085388,0.,0.0203607675478933));
#9929=DIRECTION('',(0.,1.,0.));
#9930=DIRECTION('center_axis',(-0.0610485395348597,0.,0.998134798421867));
#9931=DIRECTION('ref_axis',(0.998134798421867,0.,0.0610485395348597));
#9932=DIRECTION('',(0.998134798421867,0.,0.0610485395348597));
#9933=DIRECTION('',(0.,1.,0.));
#9934=DIRECTION('center_axis',(-0.101635078182801,0.,0.994821748296033));
#9935=DIRECTION('ref_axis',(0.994821748296033,0.,0.101635078182801));
#9936=DIRECTION('',(0.994821748296033,0.,0.101635078182801));
#9937=DIRECTION('',(0.,1.,0.));
#9938=DIRECTION('center_axis',(-0.992546151641322,0.,-0.121869343405148));
#9939=DIRECTION('ref_axis',(-0.121869343405148,0.,0.992546151641322));
#9940=DIRECTION('',(-0.121869343405148,0.,0.992546151641322));
#9941=DIRECTION('center_axis',(0.,1.,0.));
#9942=DIRECTION('ref_axis',(-1.,0.,-6.10622663543836E-16));
#9943=DIRECTION('',(0.,0.,1.));
#9944=DIRECTION('',(1.,0.,0.));
#9945=DIRECTION('',(0.,0.,1.));
#9946=DIRECTION('',(1.,0.,0.));
#9947=DIRECTION('',(0.,0.,1.));
#9948=DIRECTION('',(1.,0.,0.));
#9949=DIRECTION('axis',(0.,0.,1.));
#9950=DIRECTION('refdir',(1.,0.,0.));
#9951=DIRECTION('center_axis',(0.866025403784439,0.,-0.5));
#9952=DIRECTION('ref_axis',(0.5,0.,0.866025403784439));
#9953=DIRECTION('',(0.5,0.,0.866025403784439));
#9954=DIRECTION('',(0.,-1.,0.));
#9955=DIRECTION('',(0.5,0.,0.866025403784439));
#9956=DIRECTION('',(0.,-1.,0.));
#9957=DIRECTION('center_axis',(1.92296268638356E-16,0.,-1.));
#9958=DIRECTION('ref_axis',(1.,0.,1.92296268638356E-16));
#9959=DIRECTION('',(1.,0.,1.92296268638356E-16));
#9960=DIRECTION('',(0.,-1.,0.));
#9961=DIRECTION('',(1.,0.,1.92296268638356E-16));
#9962=DIRECTION('center_axis',(-0.866025403784439,0.,-0.5));
#9963=DIRECTION('ref_axis',(0.5,0.,-0.866025403784439));
#9964=DIRECTION('',(0.5,0.,-0.866025403784439));
#9965=DIRECTION('',(0.,-1.,0.));
#9966=DIRECTION('',(0.5,0.,-0.866025403784438));
#9967=DIRECTION('center_axis',(-0.866025403784439,0.,0.5));
#9968=DIRECTION('ref_axis',(-0.5,0.,-0.866025403784439));
#9969=DIRECTION('',(-0.5,0.,-0.866025403784439));
#9970=DIRECTION('',(0.,-1.,0.));
#9971=DIRECTION('',(-0.5,0.,-0.866025403784439));
#9972=DIRECTION('center_axis',(-1.92296268638356E-16,0.,1.));
#9973=DIRECTION('ref_axis',(-1.,0.,-1.92296268638356E-16));
#9974=DIRECTION('',(-1.,0.,-1.92296268638356E-16));
#9975=DIRECTION('',(0.,-1.,0.));
#9976=DIRECTION('',(-1.,0.,-1.92296268638356E-16));
#9977=DIRECTION('center_axis',(0.866025403784439,0.,0.5));
#9978=DIRECTION('ref_axis',(-0.5,0.,0.866025403784439));
#9979=DIRECTION('',(-0.5,0.,0.866025403784439));
#9980=DIRECTION('',(-0.5,0.,0.866025403784439));
#9981=DIRECTION('center_axis',(0.,-1.,0.));
#9982=DIRECTION('ref_axis',(0.,0.,-1.));
#9983=DIRECTION('center_axis',(0.,1.,0.));
#9984=DIRECTION('ref_axis',(0.,0.,1.));
#9985=DIRECTION('center_axis',(0.,-1.,0.));
#9986=DIRECTION('ref_axis',(1.,0.,0.));
#9987=DIRECTION('center_axis',(0.,-1.,0.));
#9988=DIRECTION('ref_axis',(1.,0.,0.));
#9989=DIRECTION('center_axis',(0.,-1.,0.));
#9990=DIRECTION('ref_axis',(1.,0.,0.));
#9991=DIRECTION('',(0.707106781186547,0.707106781186548,8.65956056235493E-17));
#9992=DIRECTION('center_axis',(0.,-1.,0.));
#9993=DIRECTION('ref_axis',(1.,0.,0.));
#9994=DIRECTION('center_axis',(0.,1.,0.));
#9995=DIRECTION('ref_axis',(1.,0.,0.));
#9996=DIRECTION('',(0.,1.,0.));
#9997=DIRECTION('center_axis',(0.,1.,0.));
#9998=DIRECTION('ref_axis',(1.,0.,0.));
#9999=DIRECTION('center_axis',(0.,-1.,0.));
#10000=DIRECTION('ref_axis',(1.,0.,0.));
#10001=DIRECTION('',(-0.707106781186547,0.707106781186548,-8.65956056235493E-17));
#10002=DIRECTION('center_axis',(0.,-1.,0.));
#10003=DIRECTION('ref_axis',(0.,0.,-1.));
#10004=DIRECTION('',(0.,0.,1.));
#10005=DIRECTION('',(1.,0.,0.));
#10006=DIRECTION('',(0.,0.,1.));
#10007=DIRECTION('',(1.,0.,0.));
#10008=DIRECTION('',(0.,0.,1.));
#10009=DIRECTION('',(1.,0.,0.));
#10010=DIRECTION('',(0.,0.,1.));
#10011=DIRECTION('',(1.,0.,0.));
#10012=DIRECTION('',(0.,-1.,2.22044604925031E-16));
#10013=DIRECTION('',(1.,0.,0.));
#10014=DIRECTION('',(0.,-1.,2.22044604925031E-16));
#10015=DIRECTION('',(1.,0.,0.));
#10016=DIRECTION('',(0.,0.,1.));
#10017=DIRECTION('',(2.22044604925031E-16,-1.,0.));
#10018=DIRECTION('',(0.,0.,1.));
#10019=DIRECTION('',(1.,0.,0.));
#10020=DIRECTION('',(0.,-1.,2.22044604925031E-16));
#10021=DIRECTION('',(1.,0.,0.));
#10022=DIRECTION('',(0.,-1.,2.22044604925031E-16));
#10023=DIRECTION('',(1.,0.,0.));
#10024=DIRECTION('',(0.,0.,1.));
#10025=DIRECTION('',(2.22044604925031E-16,-1.,0.));
#10026=DIRECTION('',(0.,0.,1.));
#10027=DIRECTION('',(1.,0.,0.));
#10028=DIRECTION('',(0.,0.,1.));
#10029=DIRECTION('',(2.22044604925031E-16,-1.,0.));
#10030=DIRECTION('',(0.,0.,1.));
#10031=DIRECTION('',(1.,0.,0.));
#10032=DIRECTION('',(0.,0.,1.));
#10033=DIRECTION('',(2.22044604925031E-16,-1.,0.));
#10034=DIRECTION('',(0.,0.,1.));
#10035=DIRECTION('',(1.,0.,0.));
#10036=DIRECTION('',(0.,-1.,0.));
#10037=DIRECTION('',(1.,0.,0.));
#10038=DIRECTION('',(0.,-1.,0.));
#10039=DIRECTION('',(0.5,0.,-0.866025403784439));
#10040=CARTESIAN_POINT('',(0.,0.,0.));
#10041=CARTESIAN_POINT('',(0.,0.,0.));
#10042=CARTESIAN_POINT('Origin',(1.6,-9.,-0.1));
#10043=CARTESIAN_POINT('',(1.39,-9.,0.));
#10044=CARTESIAN_POINT('Origin',(1.6,-9.,0.));
#10045=CARTESIAN_POINT('',(1.39,-9.,1.2));
#10046=CARTESIAN_POINT('',(1.39,-9.,-0.1));
#10047=CARTESIAN_POINT('Origin',(1.6,-9.,1.2));
#10048=CARTESIAN_POINT('Origin',(-1.6,9.,-0.1));
#10049=CARTESIAN_POINT('',(-1.81,9.,0.));
#10050=CARTESIAN_POINT('Origin',(-1.6,9.,0.));
#10051=CARTESIAN_POINT('',(-1.81,9.,1.2));
#10052=CARTESIAN_POINT('',(-1.81,9.,-0.1));
#10053=CARTESIAN_POINT('Origin',(-1.6,9.,1.2));
#10054=CARTESIAN_POINT('Origin',(-1.6,-9.,-0.1));
#10055=CARTESIAN_POINT('',(-1.81,-9.,0.));
#10056=CARTESIAN_POINT('Origin',(-1.6,-9.,0.));
#10057=CARTESIAN_POINT('',(-1.81,-9.,1.2));
#10058=CARTESIAN_POINT('',(-1.81,-9.,-0.1));
#10059=CARTESIAN_POINT('Origin',(-1.6,-9.,1.2));
#10060=CARTESIAN_POINT('Origin',(1.6,9.,-0.1));
#10061=CARTESIAN_POINT('',(1.39,9.,0.));
#10062=CARTESIAN_POINT('Origin',(1.6,9.,0.));
#10063=CARTESIAN_POINT('',(1.39,9.,1.2));
#10064=CARTESIAN_POINT('',(1.39,9.,-0.1));
#10065=CARTESIAN_POINT('Origin',(1.6,9.,1.2));
#10066=CARTESIAN_POINT('Origin',(4.,14.5,0.));
#10067=CARTESIAN_POINT('',(4.,14.5,0.));
#10068=CARTESIAN_POINT('',(-4.,14.5,0.));
#10069=CARTESIAN_POINT('',(4.,14.5,0.));
#10070=CARTESIAN_POINT('',(-4.,14.5,1.2));
#10071=CARTESIAN_POINT('',(-4.,14.5,0.));
#10072=CARTESIAN_POINT('',(4.,14.5,1.2));
#10073=CARTESIAN_POINT('',(4.,14.5,1.2));
#10074=CARTESIAN_POINT('',(4.,14.5,0.));
#10075=CARTESIAN_POINT('Origin',(4.,-14.5,0.));
#10076=CARTESIAN_POINT('',(4.,-14.5,0.));
#10077=CARTESIAN_POINT('',(4.,-14.5,0.));
#10078=CARTESIAN_POINT('',(4.,-14.5,1.2));
#10079=CARTESIAN_POINT('',(4.,-14.5,1.2));
#10080=CARTESIAN_POINT('',(4.,-14.5,0.));
#10081=CARTESIAN_POINT('Origin',(-4.,-14.5,0.));
#10082=CARTESIAN_POINT('',(-4.,-14.5,0.));
#10083=CARTESIAN_POINT('',(-4.,-14.5,0.));
#10084=CARTESIAN_POINT('',(-4.,-14.5,1.2));
#10085=CARTESIAN_POINT('',(-4.,-14.5,1.2));
#10086=CARTESIAN_POINT('',(-4.,-14.5,0.));
#10087=CARTESIAN_POINT('Origin',(-4.,14.5,0.));
#10088=CARTESIAN_POINT('',(-4.,14.5,0.));
#10089=CARTESIAN_POINT('',(-4.,14.5,1.2));
#10090=CARTESIAN_POINT('Origin',(0.,0.,1.2));
#10091=CARTESIAN_POINT('Origin',(0.,0.,0.));
#10092=CARTESIAN_POINT('',(0.,0.,0.));
#10093=CARTESIAN_POINT('Origin',(0.,-13.,3.5));
#10094=CARTESIAN_POINT('',(-0.6,-0.399999999999999,3.5));
#10095=CARTESIAN_POINT('Origin',(0.,-0.399999999999999,3.5));
#10096=CARTESIAN_POINT('',(-0.6,-13.,3.5));
#10097=CARTESIAN_POINT('',(-0.6,-13.,3.5));
#10098=CARTESIAN_POINT('Origin',(0.,-13.,3.5));
#10099=CARTESIAN_POINT('Origin',(0.,-0.399999999999999,3.5));
#10100=CARTESIAN_POINT('Origin',(0.,-13.,3.5));
#10101=CARTESIAN_POINT('',(0.,0.,0.));
#10102=CARTESIAN_POINT('Origin',(0.,0.4,3.5));
#10103=CARTESIAN_POINT('',(-0.6,13.,3.5));
#10104=CARTESIAN_POINT('Origin',(0.,13.,3.5));
#10105=CARTESIAN_POINT('',(-0.6,0.4,3.5));
#10106=CARTESIAN_POINT('',(-0.6,0.4,3.5));
#10107=CARTESIAN_POINT('Origin',(0.,0.4,3.5));
#10108=CARTESIAN_POINT('Origin',(0.,13.,3.5));
#10109=CARTESIAN_POINT('Origin',(0.,0.4,3.5));
#10110=CARTESIAN_POINT('',(0.,0.,0.));
#10111=CARTESIAN_POINT('Origin',(-1.6,0.,1.3));
#10112=CARTESIAN_POINT('',(-1.2,0.340036762718386,1.3));
#10113=CARTESIAN_POINT('',(-1.2,-0.340036762718386,1.3));
#10114=CARTESIAN_POINT('',(-1.2,0.,1.3));
#10115=CARTESIAN_POINT('Origin',(-1.6,0.,1.3));
#10116=CARTESIAN_POINT('Origin',(-1.6,0.,0.6));
#10117=CARTESIAN_POINT('',(-1.2,0.340036762718386,0.6));
#10118=CARTESIAN_POINT('',(-1.2,0.340036762718386,0.6));
#10119=CARTESIAN_POINT('',(-1.2,-0.340036762718386,0.6));
#10120=CARTESIAN_POINT('Origin',(-1.6,0.,0.6));
#10121=CARTESIAN_POINT('',(-1.2,-0.340036762718386,0.6));
#10122=CARTESIAN_POINT('Origin',(1.6,0.,0.6));
#10123=CARTESIAN_POINT('',(1.2,0.340036762718386,1.3));
#10124=CARTESIAN_POINT('',(1.2,0.340036762718386,0.6));
#10125=CARTESIAN_POINT('',(1.2,0.340036762718386,0.6));
#10126=CARTESIAN_POINT('',(1.2,-0.340036762718386,1.3));
#10127=CARTESIAN_POINT('Origin',(1.6,0.,1.3));
#10128=CARTESIAN_POINT('',(1.2,-0.340036762718386,0.6));
#10129=CARTESIAN_POINT('',(1.2,-0.340036762718386,0.6));
#10130=CARTESIAN_POINT('Origin',(1.6,0.,0.6));
#10131=CARTESIAN_POINT('Origin',(1.6,0.,1.3));
#10132=CARTESIAN_POINT('',(1.2,0.,1.3));
#10133=CARTESIAN_POINT('Origin',(-2.1,0.,0.6));
#10134=CARTESIAN_POINT('',(-1.2,0.7,0.6));
#10135=CARTESIAN_POINT('',(-1.2,0.,0.6));
#10136=CARTESIAN_POINT('',(-2.1,0.7,0.6));
#10137=CARTESIAN_POINT('',(-1.2,0.7,0.6));
#10138=CARTESIAN_POINT('',(-2.1,-0.7,0.6));
#10139=CARTESIAN_POINT('',(-2.1,0.,0.6));
#10140=CARTESIAN_POINT('',(-1.2,-0.7,0.6));
#10141=CARTESIAN_POINT('',(-1.2,-0.7,0.6));
#10142=CARTESIAN_POINT('',(-1.2,0.,0.6));
#10143=CARTESIAN_POINT('',(-1.875,3.36777869765522E-17,0.6));
#10144=CARTESIAN_POINT('Origin',(-1.6,0.,0.6));
#10145=CARTESIAN_POINT('Origin',(-1.2,0.,0.6));
#10146=CARTESIAN_POINT('',(-1.2,-0.7,3.75));
#10147=CARTESIAN_POINT('',(-1.2,-0.7,3.75));
#10148=CARTESIAN_POINT('',(-1.2,0.7,3.75));
#10149=CARTESIAN_POINT('',(-1.2,0.,3.75));
#10150=CARTESIAN_POINT('',(-1.2,0.7,3.75));
#10151=CARTESIAN_POINT('',(-1.2,-2.02066721859313E-17,3.515));
#10152=CARTESIAN_POINT('Origin',(-1.2,0.,3.35));
#10153=CARTESIAN_POINT('Origin',(1.2,0.,0.6));
#10154=CARTESIAN_POINT('',(2.1,-0.7,0.6));
#10155=CARTESIAN_POINT('',(2.1,0.7,0.6));
#10156=CARTESIAN_POINT('',(2.1,0.,0.6));
#10157=CARTESIAN_POINT('',(1.2,0.7,0.6));
#10158=CARTESIAN_POINT('',(2.1,0.7,0.6));
#10159=CARTESIAN_POINT('',(1.2,0.,0.6));
#10160=CARTESIAN_POINT('',(1.2,-0.7,0.6));
#10161=CARTESIAN_POINT('',(1.2,0.,0.6));
#10162=CARTESIAN_POINT('',(2.1,-0.7,0.6));
#10163=CARTESIAN_POINT('',(1.325,3.36777869765522E-17,0.6));
#10164=CARTESIAN_POINT('Origin',(1.6,0.,0.6));
#10165=CARTESIAN_POINT('Origin',(0.1,0.,3.35));
#10166=CARTESIAN_POINT('',(0.1,-2.75545529808155E-17,3.575));
#10167=CARTESIAN_POINT('Origin',(0.1,0.,3.35));
#10168=CARTESIAN_POINT('',(1.2,2.75545529808155E-17,3.575));
#10169=CARTESIAN_POINT('',(0.1,-2.75545529808155E-17,3.575));
#10170=CARTESIAN_POINT('Origin',(1.2,0.,3.35));
#10171=CARTESIAN_POINT('Origin',(0.,0.,3.35));
#10172=CARTESIAN_POINT('',(-0.1,2.02066721859313E-17,3.515));
#10173=CARTESIAN_POINT('',(0.,-2.02066721859313E-17,3.515));
#10174=CARTESIAN_POINT('Origin',(-0.1,0.,3.35));
#10175=CARTESIAN_POINT('Origin',(-1.6,0.,-0.05));
#10176=CARTESIAN_POINT('',(-1.875,-3.36777869765522E-17,0.));
#10177=CARTESIAN_POINT('Origin',(-1.6,0.,0.));
#10178=CARTESIAN_POINT('',(-1.875,-3.36777869765522E-17,-0.05));
#10179=CARTESIAN_POINT('Origin',(1.6,0.,-0.05));
#10180=CARTESIAN_POINT('',(1.325,-3.36777869765522E-17,0.));
#10181=CARTESIAN_POINT('Origin',(1.6,0.,0.));
#10182=CARTESIAN_POINT('',(1.325,-3.36777869765522E-17,-0.05));
#10183=CARTESIAN_POINT('Origin',(0.,0.,2.3));
#10184=CARTESIAN_POINT('',(-0.6,-0.7,2.3));
#10185=CARTESIAN_POINT('Origin',(0.,-0.7,2.3));
#10186=CARTESIAN_POINT('',(-0.6,0.7,2.3));
#10187=CARTESIAN_POINT('',(-0.6,0.,2.3));
#10188=CARTESIAN_POINT('Origin',(0.,0.7,2.3));
#10189=CARTESIAN_POINT('Origin',(0.,-0.7,1.875));
#10190=CARTESIAN_POINT('',(-2.1,-0.7,0.));
#10191=CARTESIAN_POINT('',(-2.1,-0.7,0.6));
#10192=CARTESIAN_POINT('',(2.1,-0.7,0.));
#10193=CARTESIAN_POINT('',(-2.1,-0.7,0.));
#10194=CARTESIAN_POINT('',(2.1,-0.7,0.));
#10195=CARTESIAN_POINT('',(1.2,-0.7,3.75));
#10196=CARTESIAN_POINT('',(1.2,-0.7,0.6));
#10197=CARTESIAN_POINT('',(0.1,-0.7,3.75));
#10198=CARTESIAN_POINT('',(1.2,-0.7,3.75));
#10199=CARTESIAN_POINT('',(0.1,-0.7,2.95));
#10200=CARTESIAN_POINT('',(0.1,-0.7,3.75));
#10201=CARTESIAN_POINT('',(-0.1,-0.7,2.95));
#10202=CARTESIAN_POINT('',(0.1,-0.7,2.95));
#10203=CARTESIAN_POINT('',(-0.1,-0.7,3.75));
#10204=CARTESIAN_POINT('',(-0.1,-0.7,2.95));
#10205=CARTESIAN_POINT('',(-0.1,-0.7,3.75));
#10206=CARTESIAN_POINT('Origin',(-2.1,0.,0.));
#10207=CARTESIAN_POINT('',(-2.1,0.7,0.));
#10208=CARTESIAN_POINT('',(-2.1,0.7,0.6));
#10209=CARTESIAN_POINT('',(-2.1,0.,0.));
#10210=CARTESIAN_POINT('Origin',(2.1,0.,0.));
#10211=CARTESIAN_POINT('',(2.1,0.7,0.));
#10212=CARTESIAN_POINT('',(-2.1,0.7,0.));
#10213=CARTESIAN_POINT('',(2.1,0.,0.));
#10214=CARTESIAN_POINT('Origin',(2.1,0.,0.6));
#10215=CARTESIAN_POINT('',(2.1,0.7,0.));
#10216=CARTESIAN_POINT('Origin',(1.2,0.,3.75));
#10217=CARTESIAN_POINT('',(1.2,0.7,3.75));
#10218=CARTESIAN_POINT('',(1.2,0.7,0.6));
#10219=CARTESIAN_POINT('',(1.2,0.,3.75));
#10220=CARTESIAN_POINT('Origin',(0.1,0.,3.75));
#10221=CARTESIAN_POINT('',(0.1,0.7,3.75));
#10222=CARTESIAN_POINT('',(1.2,0.7,3.75));
#10223=CARTESIAN_POINT('',(0.1,0.,3.75));
#10224=CARTESIAN_POINT('Origin',(0.1,0.,2.95));
#10225=CARTESIAN_POINT('',(0.1,0.7,2.95));
#10226=CARTESIAN_POINT('',(0.1,0.7,3.75));
#10227=CARTESIAN_POINT('',(0.1,0.,2.95));
#10228=CARTESIAN_POINT('Origin',(-0.1,0.,2.95));
#10229=CARTESIAN_POINT('',(-0.1,0.7,2.95));
#10230=CARTESIAN_POINT('',(0.1,0.7,2.95));
#10231=CARTESIAN_POINT('',(-0.1,0.,2.95));
#10232=CARTESIAN_POINT('Origin',(-0.1,0.,3.75));
#10233=CARTESIAN_POINT('',(-0.1,0.7,3.75));
#10234=CARTESIAN_POINT('',(-0.1,0.7,2.95));
#10235=CARTESIAN_POINT('',(-0.1,0.,3.75));
#10236=CARTESIAN_POINT('Origin',(-1.2,0.,3.75));
#10237=CARTESIAN_POINT('',(-0.1,0.7,3.75));
#10238=CARTESIAN_POINT('Origin',(0.,0.7,1.875));
#10239=CARTESIAN_POINT('',(0.,0.,0.));
#10240=CARTESIAN_POINT('Origin',(0.115470053837925,-0.5,-0.2));
#10241=CARTESIAN_POINT('',(0.23094010767585,-0.5,0.));
#10242=CARTESIAN_POINT('',(0.115470053837925,-0.5,-0.2));
#10243=CARTESIAN_POINT('',(0.23094010767585,-0.5,0.));
#10244=CARTESIAN_POINT('',(0.115470053837925,-0.8,-0.2));
#10245=CARTESIAN_POINT('',(0.115470053837925,-0.5,-0.2));
#10246=CARTESIAN_POINT('',(0.23094010767585,-0.8,0.));
#10247=CARTESIAN_POINT('',(0.23094010767585,-0.8,0.));
#10248=CARTESIAN_POINT('',(0.23094010767585,-0.5,0.));
#10249=CARTESIAN_POINT('Origin',(-0.115470053837925,-0.5,-0.2));
#10250=CARTESIAN_POINT('',(-0.115470053837925,-0.5,-0.2));
#10251=CARTESIAN_POINT('',(0.115470053837925,-0.5,-0.2));
#10252=CARTESIAN_POINT('',(-0.115470053837925,-0.8,-0.2));
#10253=CARTESIAN_POINT('',(-0.115470053837925,-0.5,-0.2));
#10254=CARTESIAN_POINT('',(0.115470053837925,-0.8,-0.2));
#10255=CARTESIAN_POINT('Origin',(-0.23094010767585,-0.5,-2.77555756156289E-17));
#10256=CARTESIAN_POINT('',(-0.23094010767585,-0.5,-2.82820063659975E-17));
#10257=CARTESIAN_POINT('',(-0.115470053837925,-0.5,-0.2));
#10258=CARTESIAN_POINT('',(-0.23094010767585,-0.8,-2.77555756156289E-17));
#10259=CARTESIAN_POINT('',(-0.23094010767585,-0.5,-2.82820063659975E-17));
#10260=CARTESIAN_POINT('',(-0.115470053837925,-0.8,-0.2));
#10261=CARTESIAN_POINT('Origin',(-0.115470053837925,-0.5,0.2));
#10262=CARTESIAN_POINT('',(-0.115470053837925,-0.5,0.2));
#10263=CARTESIAN_POINT('',(-0.23094010767585,-0.5,-2.82820063659975E-17));
#10264=CARTESIAN_POINT('',(-0.115470053837925,-0.8,0.2));
#10265=CARTESIAN_POINT('',(-0.115470053837925,-0.5,0.2));
#10266=CARTESIAN_POINT('',(-0.23094010767585,-0.8,-2.82820063659975E-17));
#10267=CARTESIAN_POINT('Origin',(0.115470053837925,-0.5,0.2));
#10268=CARTESIAN_POINT('',(0.115470053837925,-0.5,0.2));
#10269=CARTESIAN_POINT('',(-0.115470053837925,-0.5,0.2));
#10270=CARTESIAN_POINT('',(0.115470053837925,-0.8,0.2));
#10271=CARTESIAN_POINT('',(0.115470053837925,-0.5,0.2));
#10272=CARTESIAN_POINT('',(-0.115470053837925,-0.8,0.2));
#10273=CARTESIAN_POINT('Origin',(0.23094010767585,-0.5,0.));
#10274=CARTESIAN_POINT('',(0.115470053837925,-0.5,0.2));
#10275=CARTESIAN_POINT('',(0.115470053837925,-0.8,0.2));
#10276=CARTESIAN_POINT('Origin',(0.,-0.5,0.));
#10277=CARTESIAN_POINT('Origin',(0.,-0.8,0.));
#10278=CARTESIAN_POINT('Origin',(0.,-1.4,0.));
#10279=CARTESIAN_POINT('',(-0.24505,-1.4,3.00099698131059E-17));
#10280=CARTESIAN_POINT('Origin',(0.,-1.4,0.));
#10281=CARTESIAN_POINT('Origin',(0.375,0.5,0.));
#10282=CARTESIAN_POINT('',(-0.375,0.5,-4.59242549680257E-17));
#10283=CARTESIAN_POINT('Origin',(0.,0.5,0.));
#10284=CARTESIAN_POINT('Origin',(0.,0.475,0.));
#10285=CARTESIAN_POINT('',(-0.425,0.45,-5.20474889637625E-17));
#10286=CARTESIAN_POINT('Origin',(0.,0.45,0.));
#10287=CARTESIAN_POINT('',(-0.4,0.475,-4.89858719658941E-17));
#10288=CARTESIAN_POINT('Origin',(0.,0.24,0.));
#10289=CARTESIAN_POINT('',(-0.425,0.0299999999999998,-5.20474889637625E-17));
#10290=CARTESIAN_POINT('Origin',(0.,0.0299999999999998,0.));
#10291=CARTESIAN_POINT('',(-0.425,0.24,-5.20474889637625E-17));
#10292=CARTESIAN_POINT('Origin',(0.,0.0150000000000001,0.));
#10293=CARTESIAN_POINT('',(-0.395,4.85722573273506E-17,-4.83735485663204E-17));
#10294=CARTESIAN_POINT('Origin',(0.,0.,0.));
#10295=CARTESIAN_POINT('',(-0.41,0.0150000000000001,-5.02105187650415E-17));
#10296=CARTESIAN_POINT('Origin',(0.27,0.,0.));
#10297=CARTESIAN_POINT('',(-0.27,0.,-3.30654635769785E-17));
#10298=CARTESIAN_POINT('Origin',(0.,0.,0.));
#10299=CARTESIAN_POINT('Origin',(0.,-0.02,0.));
#10300=CARTESIAN_POINT('',(-0.24505,-0.0498999999999999,3.00099698131059E-17));
#10301=CARTESIAN_POINT('Origin',(0.,-0.0498999999999999,0.));
#10302=CARTESIAN_POINT('',(-0.26,-0.02,-3.18408167778312E-17));
#10303=CARTESIAN_POINT('Origin',(0.,-0.995,0.));
#10304=CARTESIAN_POINT('',(-0.24505,-0.995,-3.00099698131059E-17));
#10305=CARTESIAN_POINT('',(0.,0.,0.));
#10306=CARTESIAN_POINT('Origin',(0.3,0.4,0.));
#10307=CARTESIAN_POINT('',(-0.3,0.4,-3.67394039744206E-17));
#10308=CARTESIAN_POINT('Origin',(0.,0.4,0.));
#10309=CARTESIAN_POINT('Origin',(0.,0.375,0.));
#10310=CARTESIAN_POINT('',(-0.35,0.35,-4.28626379701573E-17));
#10311=CARTESIAN_POINT('Origin',(0.,0.35,0.));
#10312=CARTESIAN_POINT('',(-0.325,0.375,-3.9801020972289E-17));
#10313=CARTESIAN_POINT('Origin',(0.,0.19,0.));
#10314=CARTESIAN_POINT('',(-0.35,0.03,-4.28626379701574E-17));
#10315=CARTESIAN_POINT('Origin',(0.,0.03,0.));
#10316=CARTESIAN_POINT('',(-0.35,0.19,-4.28626379701574E-17));
#10317=CARTESIAN_POINT('Origin',(0.,0.0149999999999999,0.));
#10318=CARTESIAN_POINT('',(-0.32,-3.29597460435593E-17,-3.91886975727153E-17));
#10319=CARTESIAN_POINT('Origin',(0.,0.,0.));
#10320=CARTESIAN_POINT('',(-0.335,0.0149999999999999,-4.10256677714363E-17));
#10321=CARTESIAN_POINT('Origin',(0.22,0.,0.));
#10322=CARTESIAN_POINT('',(-0.22,-6.93889390390723E-18,-2.69422295812418E-17));
#10323=CARTESIAN_POINT('Origin',(0.,0.,0.));
#10324=CARTESIAN_POINT('Origin',(0.,-0.02,0.));
#10325=CARTESIAN_POINT('',(-0.1954,-0.0492,2.39295984553393E-17));
#10326=CARTESIAN_POINT('Origin',(0.,-0.0492,0.));
#10327=CARTESIAN_POINT('',(-0.21,-0.02,-2.57175827820944E-17));
#10328=CARTESIAN_POINT('Origin',(0.,-0.8,0.));
#10329=CARTESIAN_POINT('',(-0.1954,-1.5646,2.39295984553393E-17));
#10330=CARTESIAN_POINT('Origin',(0.,-1.5646,0.));
#10331=CARTESIAN_POINT('',(-0.1954,-0.8,-2.39295984553393E-17));
#10332=CARTESIAN_POINT('Origin',(0.,-1.58,0.));
#10333=CARTESIAN_POINT('',(-0.16,-1.6,-1.95943487863577E-17));
#10334=CARTESIAN_POINT('Origin',(0.,-1.6,0.));
#10335=CARTESIAN_POINT('',(-0.18,-1.58,-2.20436423846524E-17));
#10336=CARTESIAN_POINT('Origin',(0.,-1.6,0.));
#10337=CARTESIAN_POINT('Origin',(0.0866025403784439,-0.4,-0.15));
#10338=CARTESIAN_POINT('',(0.173205080756888,-0.4,0.));
#10339=CARTESIAN_POINT('',(0.0866025403784439,-0.4,-0.15));
#10340=CARTESIAN_POINT('',(0.173205080756888,-0.4,0.));
#10341=CARTESIAN_POINT('',(0.0866025403784439,-0.64,-0.15));
#10342=CARTESIAN_POINT('',(0.0866025403784439,-0.4,-0.15));
#10343=CARTESIAN_POINT('',(0.173205080756888,-0.64,0.));
#10344=CARTESIAN_POINT('',(0.173205080756888,-0.64,0.));
#10345=CARTESIAN_POINT('',(0.173205080756888,-0.4,0.));
#10346=CARTESIAN_POINT('Origin',(-0.0866025403784438,-0.4,-0.15));
#10347=CARTESIAN_POINT('',(-0.0866025403784438,-0.4,-0.15));
#10348=CARTESIAN_POINT('',(0.0866025403784439,-0.4,-0.15));
#10349=CARTESIAN_POINT('',(-0.0866025403784438,-0.64,-0.15));
#10350=CARTESIAN_POINT('',(-0.0866025403784438,-0.4,-0.15));
#10351=CARTESIAN_POINT('',(0.0866025403784439,-0.64,-0.15));
#10352=CARTESIAN_POINT('Origin',(-0.173205080756888,-0.4,-2.77555756156289E-17));
#10353=CARTESIAN_POINT('',(-0.173205080756888,-0.4,-2.12115047744981E-17));
#10354=CARTESIAN_POINT('',(-0.0866025403784438,-0.4,-0.15));
#10355=CARTESIAN_POINT('',(-0.173205080756888,-0.64,-2.77555756156289E-17));
#10356=CARTESIAN_POINT('',(-0.173205080756888,-0.4,-2.12115047744981E-17));
#10357=CARTESIAN_POINT('',(-0.0866025403784438,-0.64,-0.15));
#10358=CARTESIAN_POINT('Origin',(-0.0866025403784439,-0.4,0.15));
#10359=CARTESIAN_POINT('',(-0.0866025403784439,-0.4,0.15));
#10360=CARTESIAN_POINT('',(-0.173205080756888,-0.4,-2.12115047744981E-17));
#10361=CARTESIAN_POINT('',(-0.0866025403784439,-0.64,0.15));
#10362=CARTESIAN_POINT('',(-0.0866025403784439,-0.4,0.15));
#10363=CARTESIAN_POINT('',(-0.173205080756888,-0.64,-2.12115047744981E-17));
#10364=CARTESIAN_POINT('Origin',(0.0866025403784439,-0.4,0.15));
#10365=CARTESIAN_POINT('',(0.0866025403784439,-0.4,0.15));
#10366=CARTESIAN_POINT('',(-0.0866025403784439,-0.4,0.15));
#10367=CARTESIAN_POINT('',(0.0866025403784439,-0.64,0.15));
#10368=CARTESIAN_POINT('',(0.0866025403784439,-0.4,0.15));
#10369=CARTESIAN_POINT('',(-0.0866025403784439,-0.64,0.15));
#10370=CARTESIAN_POINT('Origin',(0.173205080756888,-0.4,0.));
#10371=CARTESIAN_POINT('',(0.0866025403784439,-0.4,0.15));
#10372=CARTESIAN_POINT('',(0.0866025403784439,-0.64,0.15));
#10373=CARTESIAN_POINT('Origin',(0.,-0.4,-2.77555756156289E-17));
#10374=CARTESIAN_POINT('Origin',(0.,-0.64,-2.77555756156289E-17));
#10375=CARTESIAN_POINT('',(0.,0.,0.));
#10376=CARTESIAN_POINT('Origin',(0.5,0.6,0.));
#10377=CARTESIAN_POINT('',(0.561411711669787,0.6,0.2117));
#10378=CARTESIAN_POINT('Ctrl Pts',(0.561411711669787,0.6,0.2117));
#10379=CARTESIAN_POINT('Ctrl Pts',(0.561411711669787,0.573158649069562,
0.2117));
#10380=CARTESIAN_POINT('Ctrl Pts',(0.563539297838208,0.544705001203387,
0.206288194517509));
#10381=CARTESIAN_POINT('Ctrl Pts',(0.571006257413022,0.492626080621549,
0.184616375754799));
#10382=CARTESIAN_POINT('Ctrl Pts',(0.576215579648966,0.468977868958045,
0.168366880112429));
#10383=CARTESIAN_POINT('Ctrl Pts',(0.585834170098139,0.431644140867814,
0.131033152022198));
#10384=CARTESIAN_POINT('Ctrl Pts',(0.590898115435695,0.41538619377614,0.107380608633747));
#10385=CARTESIAN_POINT('Ctrl Pts',(0.598025669508798,0.393708029332882,
0.0552854099234836));
#10386=CARTESIAN_POINT('Ctrl Pts',(0.6,0.3883,0.0268255083819855));
#10387=CARTESIAN_POINT('Ctrl Pts',(0.6,0.3883,-0.0268255083819856));
#10388=CARTESIAN_POINT('Ctrl Pts',(0.598025669508798,0.393708029332882,
-0.0552854099234837));
#10389=CARTESIAN_POINT('Ctrl Pts',(0.590898115435695,0.41538619377614,-0.107380608633747));
#10390=CARTESIAN_POINT('Ctrl Pts',(0.585834170098139,0.431644140867814,
-0.131033152022198));
#10391=CARTESIAN_POINT('Ctrl Pts',(0.576215579648966,0.468977868958045,
-0.168366880112429));
#10392=CARTESIAN_POINT('Ctrl Pts',(0.571006257413022,0.49262608062155,-0.184616375754799));
#10393=CARTESIAN_POINT('Ctrl Pts',(0.563539297838207,0.544705001203387,
-0.206288194517509));
#10394=CARTESIAN_POINT('Ctrl Pts',(0.561411711669787,0.573158649069562,
-0.2117));
#10395=CARTESIAN_POINT('Ctrl Pts',(0.561411711669787,0.626841350930438,
-0.2117));
#10396=CARTESIAN_POINT('Ctrl Pts',(0.563539297838207,0.655294998796613,
-0.206288194517509));
#10397=CARTESIAN_POINT('Ctrl Pts',(0.571006257413022,0.70737391937845,-0.184616375754799));
#10398=CARTESIAN_POINT('Ctrl Pts',(0.576215579648966,0.731022131041955,
-0.168366880112429));
#10399=CARTESIAN_POINT('Ctrl Pts',(0.585834170098139,0.768355859132186,
-0.131033152022198));
#10400=CARTESIAN_POINT('Ctrl Pts',(0.590898115435695,0.78461380622386,-0.107380608633747));
#10401=CARTESIAN_POINT('Ctrl Pts',(0.598025669508798,0.806291970667118,
-0.0552854099234837));
#10402=CARTESIAN_POINT('Ctrl Pts',(0.6,0.8117,-0.0268255083819856));
#10403=CARTESIAN_POINT('Ctrl Pts',(0.6,0.8117,0.0268255083819855));
#10404=CARTESIAN_POINT('Ctrl Pts',(0.598025669508798,0.806291970667118,
0.0552854099234837));
#10405=CARTESIAN_POINT('Ctrl Pts',(0.590898115435695,0.78461380622386,0.107380608633747));
#10406=CARTESIAN_POINT('Ctrl Pts',(0.585834170098139,0.768355859132186,
0.131033152022198));
#10407=CARTESIAN_POINT('Ctrl Pts',(0.576215579648966,0.731022131041955,
0.168366880112429));
#10408=CARTESIAN_POINT('Ctrl Pts',(0.571006257413022,0.70737391937845,0.184616375754799));
#10409=CARTESIAN_POINT('Ctrl Pts',(0.563539297838207,0.655294998796613,
0.206288194517509));
#10410=CARTESIAN_POINT('Ctrl Pts',(0.561411711669787,0.626841350930438,
0.2117));
#10411=CARTESIAN_POINT('Ctrl Pts',(0.561411711669787,0.6,0.2117));
#10412=CARTESIAN_POINT('',(1.07943647798284,0.6,0.2117));
#10413=CARTESIAN_POINT('',(0.5,0.6,0.2117));
#10414=CARTESIAN_POINT('Ctrl Pts',(1.07943647798284,0.6,0.2117));
#10415=CARTESIAN_POINT('Ctrl Pts',(1.07943647798284,0.626653802072043,0.2117));
#10416=CARTESIAN_POINT('Ctrl Pts',(1.08052600621577,0.655037401084091,0.206359582618511));
#10417=CARTESIAN_POINT('Ctrl Pts',(1.08443252298676,0.707175401021015,0.18473448130117));
#10418=CARTESIAN_POINT('Ctrl Pts',(1.08718996287164,0.730935702749545,0.168453308404839));
#10419=CARTESIAN_POINT('Ctrl Pts',(1.09234340045893,0.768452409692904,0.13093660146148));
#10420=CARTESIAN_POINT('Ctrl Pts',(1.09507838311905,0.784734286816328,0.107175917083711));
#10421=CARTESIAN_POINT('Ctrl Pts',(1.09893326276149,0.806359899102434,0.0550365908820453));
#10422=CARTESIAN_POINT('Ctrl Pts',(1.1,0.8117,0.0266525251200821));
#10423=CARTESIAN_POINT('Ctrl Pts',(1.1,0.8117,-0.0266525251200823));
#10424=CARTESIAN_POINT('Ctrl Pts',(1.09893326276149,0.806359899102434,-0.0550365908820454));
#10425=CARTESIAN_POINT('Ctrl Pts',(1.09507838311905,0.784734286816328,-0.107175917083711));
#10426=CARTESIAN_POINT('Ctrl Pts',(1.09234340045893,0.768452409692904,-0.130936601461481));
#10427=CARTESIAN_POINT('Ctrl Pts',(1.08718996287164,0.730935702749545,-0.16845330840484));
#10428=CARTESIAN_POINT('Ctrl Pts',(1.08443252298676,0.707175401021015,-0.18473448130117));
#10429=CARTESIAN_POINT('Ctrl Pts',(1.08052600621577,0.655037401084091,-0.206359582618511));
#10430=CARTESIAN_POINT('Ctrl Pts',(1.07943647798284,0.626653802072043,-0.2117));
#10431=CARTESIAN_POINT('Ctrl Pts',(1.07943647798284,0.573346197927957,-0.2117));
#10432=CARTESIAN_POINT('Ctrl Pts',(1.08052600621577,0.544962598915909,-0.206359582618511));
#10433=CARTESIAN_POINT('Ctrl Pts',(1.08443252298676,0.492824598978985,-0.18473448130117));
#10434=CARTESIAN_POINT('Ctrl Pts',(1.08718996287164,0.469064297250455,-0.168453308404839));
#10435=CARTESIAN_POINT('Ctrl Pts',(1.09234340045893,0.431547590307096,-0.13093660146148));
#10436=CARTESIAN_POINT('Ctrl Pts',(1.09507838311905,0.415265713183672,-0.107175917083711));
#10437=CARTESIAN_POINT('Ctrl Pts',(1.09893326276149,0.393640100897566,-0.0550365908820454));
#10438=CARTESIAN_POINT('Ctrl Pts',(1.1,0.3883,-0.0266525251200822));
#10439=CARTESIAN_POINT('Ctrl Pts',(1.1,0.3883,0.0266525251200823));
#10440=CARTESIAN_POINT('Ctrl Pts',(1.09893326276149,0.393640100897566,0.0550365908820454));
#10441=CARTESIAN_POINT('Ctrl Pts',(1.09507838311905,0.415265713183672,0.107175917083711));
#10442=CARTESIAN_POINT('Ctrl Pts',(1.09234340045893,0.431547590307096,0.13093660146148));
#10443=CARTESIAN_POINT('Ctrl Pts',(1.08718996287164,0.469064297250455,0.16845330840484));
#10444=CARTESIAN_POINT('Ctrl Pts',(1.08443252298676,0.492824598978985,0.18473448130117));
#10445=CARTESIAN_POINT('Ctrl Pts',(1.08052600621577,0.544962598915909,0.206359582618511));
#10446=CARTESIAN_POINT('Ctrl Pts',(1.07943647798284,0.573346197927957,0.2117));
#10447=CARTESIAN_POINT('Ctrl Pts',(1.07943647798284,0.6,0.2117));
#10448=CARTESIAN_POINT('Origin',(1.05,1.2,0.));
#10449=CARTESIAN_POINT('',(-1.05,1.2,-1.28587913910472E-16));
#10450=CARTESIAN_POINT('Origin',(0.,1.2,0.));
#10451=CARTESIAN_POINT('',(-0.6,1.2,-7.34788079488412E-17));
#10452=CARTESIAN_POINT('Origin',(0.,1.2,0.));
#10453=CARTESIAN_POINT('Origin',(0.,1.175,0.));
#10454=CARTESIAN_POINT('',(-1.1,1.15,-1.34711147906209E-16));
#10455=CARTESIAN_POINT('Origin',(0.,1.15,0.));
#10456=CARTESIAN_POINT('',(-1.075,1.175,-1.3164953090834E-16));
#10457=CARTESIAN_POINT('Origin',(0.,0.6,0.));
#10458=CARTESIAN_POINT('',(-1.1,0.05,-1.34711147906209E-16));
#10459=CARTESIAN_POINT('Origin',(0.,0.05,0.));
#10460=CARTESIAN_POINT('',(-1.1,0.6,-1.34711147906209E-16));
#10461=CARTESIAN_POINT('Origin',(0.,0.025,0.));
#10462=CARTESIAN_POINT('',(-1.05,-4.5102810375397E-17,-1.28587913910472E-16));
#10463=CARTESIAN_POINT('Origin',(0.,0.,0.));
#10464=CARTESIAN_POINT('',(-1.075,0.025,-1.3164953090834E-16));
#10465=CARTESIAN_POINT('Origin',(0.6,0.,0.));
#10466=CARTESIAN_POINT('',(-0.6,0.,-7.34788079488412E-17));
#10467=CARTESIAN_POINT('Origin',(0.,0.,0.));
#10468=CARTESIAN_POINT('Origin',(0.,0.6,0.));
#10469=CARTESIAN_POINT('',(-0.6,0.6,-7.34788079488412E-17));
#10470=CARTESIAN_POINT('',(0.,0.,0.));
#10471=CARTESIAN_POINT('',(0.,0.,0.));
#10472=CARTESIAN_POINT('Origin',(0.,-1.525,0.));
#10473=CARTESIAN_POINT('',(0.21,-1.525,0.562049819855856));
#10474=CARTESIAN_POINT('',(-0.21,-1.525,0.562049819855856));
#10475=CARTESIAN_POINT('Ctrl Pts',(0.21,-1.525,0.562049819855856));
#10476=CARTESIAN_POINT('Ctrl Pts',(0.21,-1.49837871751922,0.562049819855856));
#10477=CARTESIAN_POINT('Ctrl Pts',(0.204633348688358,-1.4701551027118,0.564140225270058));
#10478=CARTESIAN_POINT('Ctrl Pts',(0.183136586201564,-1.41849286725608,
0.571480520223595));
#10479=CARTESIAN_POINT('Ctrl Pts',(0.167016776838808,-1.39503192874046,
0.576602928616412));
#10480=CARTESIAN_POINT('Ctrl Pts',(0.129978636309075,-1.35799378821073,
0.586063715219224));
#10481=CARTESIAN_POINT('Ctrl Pts',(0.106513536936886,-1.34186587223919,
0.591045521796147));
#10482=CARTESIAN_POINT('Ctrl Pts',(0.0548356965671431,-1.32036302924048,
0.598057680137));
#10483=CARTESIAN_POINT('Ctrl Pts',(0.0266060994851219,-1.315,0.6));
#10484=CARTESIAN_POINT('Ctrl Pts',(-0.026606099485122,-1.315,0.6));
#10485=CARTESIAN_POINT('Ctrl Pts',(-0.0548356965671431,-1.32036302924048,
0.598057680137));
#10486=CARTESIAN_POINT('Ctrl Pts',(-0.106513536936886,-1.34186587223919,
0.591045521796147));
#10487=CARTESIAN_POINT('Ctrl Pts',(-0.129978636309075,-1.35799378821073,
0.586063715219224));
#10488=CARTESIAN_POINT('Ctrl Pts',(-0.167016776838808,-1.39503192874046,
0.576602928616412));
#10489=CARTESIAN_POINT('Ctrl Pts',(-0.183136586201564,-1.41849286725608,
0.571480520223595));
#10490=CARTESIAN_POINT('Ctrl Pts',(-0.204633348688358,-1.4701551027118,
0.564140225270058));
#10491=CARTESIAN_POINT('Ctrl Pts',(-0.21,-1.49837871751922,0.562049819855856));
#10492=CARTESIAN_POINT('Ctrl Pts',(-0.21,-1.525,0.562049819855856));
#10493=CARTESIAN_POINT('Ctrl Pts',(-0.21,-1.525,0.562049819855856));
#10494=CARTESIAN_POINT('Ctrl Pts',(-0.21,-1.55162128248078,0.562049819855856));
#10495=CARTESIAN_POINT('Ctrl Pts',(-0.204633348688358,-1.5798448972882,
0.564140225270058));
#10496=CARTESIAN_POINT('Ctrl Pts',(-0.183136586201564,-1.63150713274392,
0.571480520223595));
#10497=CARTESIAN_POINT('Ctrl Pts',(-0.167016776838808,-1.65496807125954,
0.576602928616412));
#10498=CARTESIAN_POINT('Ctrl Pts',(-0.129978636309075,-1.69200621178927,
0.586063715219224));
#10499=CARTESIAN_POINT('Ctrl Pts',(-0.106513536936886,-1.70813412776081,
0.591045521796147));
#10500=CARTESIAN_POINT('Ctrl Pts',(-0.0548356965671429,-1.72963697075952,
0.598057680137));
#10501=CARTESIAN_POINT('Ctrl Pts',(-0.026606099485122,-1.735,0.6));
#10502=CARTESIAN_POINT('Ctrl Pts',(0.026606099485122,-1.735,0.6));
#10503=CARTESIAN_POINT('Ctrl Pts',(0.0548356965671429,-1.72963697075952,
0.598057680137));
#10504=CARTESIAN_POINT('Ctrl Pts',(0.106513536936886,-1.70813412776081,
0.591045521796147));
#10505=CARTESIAN_POINT('Ctrl Pts',(0.129978636309075,-1.69200621178927,
0.586063715219224));
#10506=CARTESIAN_POINT('Ctrl Pts',(0.167016776838808,-1.65496807125954,
0.576602928616412));
#10507=CARTESIAN_POINT('Ctrl Pts',(0.183136586201564,-1.63150713274392,
0.571480520223595));
#10508=CARTESIAN_POINT('Ctrl Pts',(0.204633348688358,-1.5798448972882,0.564140225270058));
#10509=CARTESIAN_POINT('Ctrl Pts',(0.21,-1.55162128248078,0.562049819855856));
#10510=CARTESIAN_POINT('Ctrl Pts',(0.21,-1.525,0.562049819855856));
#10511=CARTESIAN_POINT('',(-0.21,-1.525,1.35380944006164));
#10512=CARTESIAN_POINT('',(-0.21,-1.525,0.));
#10513=CARTESIAN_POINT('Ctrl Pts',(-0.21,-1.525,1.35380944006164));
#10514=CARTESIAN_POINT('Ctrl Pts',(-0.21,-1.49858689919462,1.35380944006164));
#10515=CARTESIAN_POINT('Ctrl Pts',(-0.204712795751841,-1.47044219200607,
1.35466231450937));
#10516=CARTESIAN_POINT('Ctrl Pts',(-0.183268700413686,-1.41871515620915,
1.35772968493193));
#10517=CARTESIAN_POINT('Ctrl Pts',(-0.167114046419118,-1.39512919832077,
1.35989844568037));
#10518=CARTESIAN_POINT('Ctrl Pts',(-0.129871156089225,-1.35788630799087,
1.36395907436197));
#10519=CARTESIAN_POINT('Ctrl Pts',(-0.106285045427176,-1.34173137598416,
1.36611666311719));
#10520=CARTESIAN_POINT('Ctrl Pts',(-0.0545574871667227,-1.32028707843824,
1.36915840160825));
#10521=CARTESIAN_POINT('Ctrl Pts',(-0.026412598106597,-1.315,1.37));
#10522=CARTESIAN_POINT('Ctrl Pts',(0.0264125981065971,-1.315,1.37));
#10523=CARTESIAN_POINT('Ctrl Pts',(0.0545574871667228,-1.32028707843824,
1.36915840160825));
#10524=CARTESIAN_POINT('Ctrl Pts',(0.106285045427176,-1.34173137598416,
1.36611666311719));
#10525=CARTESIAN_POINT('Ctrl Pts',(0.129871156089225,-1.35788630799087,
1.36395907436197));
#10526=CARTESIAN_POINT('Ctrl Pts',(0.167114046419118,-1.39512919832077,
1.35989844568037));
#10527=CARTESIAN_POINT('Ctrl Pts',(0.183268700413687,-1.41871515620915,
1.35772968493193));
#10528=CARTESIAN_POINT('Ctrl Pts',(0.204712795751841,-1.47044219200607,
1.35466231450937));
#10529=CARTESIAN_POINT('Ctrl Pts',(0.21,-1.49858689919462,1.35380944006164));
#10530=CARTESIAN_POINT('Ctrl Pts',(0.21,-1.55141310080538,1.35380944006164));
#10531=CARTESIAN_POINT('Ctrl Pts',(0.204712795751841,-1.57955780799393,
1.35466231450937));
#10532=CARTESIAN_POINT('Ctrl Pts',(0.183268700413686,-1.63128484379085,
1.35772968493193));
#10533=CARTESIAN_POINT('Ctrl Pts',(0.167114046419118,-1.65487080167923,
1.35989844568037));
#10534=CARTESIAN_POINT('Ctrl Pts',(0.129871156089225,-1.69211369200913,
1.36395907436197));
#10535=CARTESIAN_POINT('Ctrl Pts',(0.106285045427176,-1.70826862401584,
1.36611666311719));
#10536=CARTESIAN_POINT('Ctrl Pts',(0.0545574871667227,-1.72971292156176,
1.36915840160825));
#10537=CARTESIAN_POINT('Ctrl Pts',(0.0264125981065971,-1.735,1.37));
#10538=CARTESIAN_POINT('Ctrl Pts',(-0.026412598106597,-1.735,1.37));
#10539=CARTESIAN_POINT('Ctrl Pts',(-0.0545574871667227,-1.72971292156176,
1.36915840160825));
#10540=CARTESIAN_POINT('Ctrl Pts',(-0.106285045427176,-1.70826862401584,
1.36611666311719));
#10541=CARTESIAN_POINT('Ctrl Pts',(-0.129871156089225,-1.69211369200912,
1.36395907436197));
#10542=CARTESIAN_POINT('Ctrl Pts',(-0.167114046419118,-1.65487080167923,
1.35989844568037));
#10543=CARTESIAN_POINT('Ctrl Pts',(-0.183268700413686,-1.63128484379085,
1.35772968493193));
#10544=CARTESIAN_POINT('Ctrl Pts',(-0.204712795751841,-1.57955780799393,
1.35466231450937));
#10545=CARTESIAN_POINT('Ctrl Pts',(-0.21,-1.55141310080538,1.35380944006164));
#10546=CARTESIAN_POINT('Ctrl Pts',(-0.21,-1.525,1.35380944006164));
#10547=CARTESIAN_POINT('Origin',(0.,0.,0.));
#10548=CARTESIAN_POINT('',(-0.6,-2.05,7.34788079488412E-17));
#10549=CARTESIAN_POINT('Origin',(0.,-2.05,0.));
#10550=CARTESIAN_POINT('',(-0.6,-1.,-7.34788079488412E-17));
#10551=CARTESIAN_POINT('',(-0.6,0.,7.34788079488412E-17));
#10552=CARTESIAN_POINT('Origin',(0.,-1.,0.));
#10553=CARTESIAN_POINT('Origin',(-0.999913779596035,-0.4,0.936521453771333));
#10554=CARTESIAN_POINT('',(-1.08689407619899,-0.4,0.834003157741947));
#10555=CARTESIAN_POINT('',(-0.999913779596035,-0.4,0.936521453771333));
#10556=CARTESIAN_POINT('',(-1.08689407619899,-0.4,0.834003157741947));
#10557=CARTESIAN_POINT('',(-1.08689407619899,-1.,0.834003157741947));
#10558=CARTESIAN_POINT('',(-1.08689407619899,-0.4,0.834003157741947));
#10559=CARTESIAN_POINT('',(-0.999913779596035,-1.,0.936521453771333));
#10560=CARTESIAN_POINT('',(-1.02165885374678,-1.,0.910891879763986));
#10561=CARTESIAN_POINT('',(-0.999913779596035,-0.4,0.936521453771333));
#10562=CARTESIAN_POINT('Origin',(-0.903303766687095,-0.4,1.0300205362462));
#10563=CARTESIAN_POINT('',(-0.903303766687095,-0.4,1.0300205362462));
#10564=CARTESIAN_POINT('',(-0.999913779596035,-0.4,0.936521453771333));
#10565=CARTESIAN_POINT('',(-0.903303766687095,-1.,1.0300205362462));
#10566=CARTESIAN_POINT('',(-0.92745626991433,-1.,1.00664576562748));
#10567=CARTESIAN_POINT('',(-0.903303766687095,-0.4,1.0300205362462));
#10568=CARTESIAN_POINT('Origin',(-0.79799444470889,-0.4,1.11359995789051));
#10569=CARTESIAN_POINT('',(-0.79799444470889,-0.4,1.11359995789051));
#10570=CARTESIAN_POINT('',(-0.903303766687095,-0.4,1.0300205362462));
#10571=CARTESIAN_POINT('',(-0.79799444470889,-1.,1.11359995789051));
#10572=CARTESIAN_POINT('',(-0.824321775203442,-1.,1.09270510247943));
#10573=CARTESIAN_POINT('',(-0.79799444470889,-0.4,1.11359995789051));
#10574=CARTESIAN_POINT('Origin',(-0.685,-0.4,1.18645480318468));
#10575=CARTESIAN_POINT('',(-0.685,-0.4,1.18645480318468));
#10576=CARTESIAN_POINT('',(-0.79799444470889,-0.4,1.11359995789051));
#10577=CARTESIAN_POINT('',(-0.685,-1.,1.18645480318468));
#10578=CARTESIAN_POINT('',(-0.713248611177222,-1.,1.16824109186114));
#10579=CARTESIAN_POINT('',(-0.685,-0.4,1.18645480318468));
#10580=CARTESIAN_POINT('Origin',(-0.565408630832021,-0.4,1.24788344014201));
#10581=CARTESIAN_POINT('',(-0.565408630832021,-0.4,1.24788344014201));
#10582=CARTESIAN_POINT('',(-0.685,-0.4,1.18645480318468));
#10583=CARTESIAN_POINT('',(-0.565408630832022,-1.,1.24788344014201));
#10584=CARTESIAN_POINT('',(-0.595306473124018,-1.,1.23252628090268));
#10585=CARTESIAN_POINT('',(-0.565408630832021,-0.4,1.24788344014201));
#10586=CARTESIAN_POINT('Origin',(-0.440372067465332,-0.4,1.29729427740829));
#10587=CARTESIAN_POINT('',(-0.440372067465332,-0.4,1.29729427740829));
#10588=CARTESIAN_POINT('',(-0.565408630832021,-0.4,1.24788344014201));
#10589=CARTESIAN_POINT('',(-0.440372067465332,-1.,1.29729427740829));
#10590=CARTESIAN_POINT('',(-0.471631208307004,-1.,1.28494156809172));
#10591=CARTESIAN_POINT('',(-0.440372067465332,-0.4,1.29729427740829));
#10592=CARTESIAN_POINT('Origin',(-0.311094480357092,-0.4,1.33421146160995));
#10593=CARTESIAN_POINT('',(-0.311094480357092,-0.4,1.33421146160995));
#10594=CARTESIAN_POINT('',(-0.440372067465332,-0.4,1.29729427740829));
#10595=CARTESIAN_POINT('',(-0.311094480357092,-1.,1.33421146160995));
#10596=CARTESIAN_POINT('',(-0.343413877134152,-1.,1.32498216555953));
#10597=CARTESIAN_POINT('',(-0.311094480357092,-0.4,1.33421146160995));
#10598=CARTESIAN_POINT('Origin',(-0.178820883341471,-0.4,1.35827946008212));
#10599=CARTESIAN_POINT('',(-0.178820883341471,-0.4,1.35827946008212));
#10600=CARTESIAN_POINT('',(-0.311094480357092,-0.4,1.33421146160995));
#10601=CARTESIAN_POINT('',(-0.178820883341471,-1.,1.35827946008212));
#10602=CARTESIAN_POINT('',(-0.211889282595376,-1.,1.35226246046408));
#10603=CARTESIAN_POINT('',(-0.178820883341471,-0.4,1.35827946008212));
#10604=CARTESIAN_POINT('Origin',(-0.104420953776042,-0.4,0.793155889099048));
#10605=CARTESIAN_POINT('',(-0.104420953776042,-0.4,0.793155889099048));
#10606=CARTESIAN_POINT('',(-0.178820883341471,-0.4,1.35827946008212));
#10607=CARTESIAN_POINT('',(-0.104420953776042,-1.,0.793155889099048));
#10608=CARTESIAN_POINT('',(-0.0522104768880209,-1.,0.396577944549524));
#10609=CARTESIAN_POINT('',(-0.104420953776042,-0.4,0.793155889099048));
#10610=CARTESIAN_POINT('Origin',(-0.181661010427499,-0.4,0.779101583421867));
#10611=CARTESIAN_POINT('',(-0.181661010427499,-0.4,0.779101583421867));
#10612=CARTESIAN_POINT('',(-0.104420953776042,-0.4,0.793155889099048));
#10613=CARTESIAN_POINT('',(-0.181661010427499,-1.,0.779101583421867));
#10614=CARTESIAN_POINT('',(-0.162350996264634,-1.,0.782615159841162));
#10615=CARTESIAN_POINT('',(-0.181661010427499,-0.4,0.779101583421867));
#10616=CARTESIAN_POINT('Origin',(-0.25715157224253,-0.4,0.757544103596084));
#10617=CARTESIAN_POINT('',(-0.25715157224253,-0.4,0.757544103596084));
#10618=CARTESIAN_POINT('',(-0.181661010427499,-0.4,0.779101583421867));
#10619=CARTESIAN_POINT('',(-0.25715157224253,-1.,0.757544103596084));
#10620=CARTESIAN_POINT('',(-0.238278931788772,-1.,0.76293347355253));
#10621=CARTESIAN_POINT('',(-0.25715157224253,-0.4,0.757544103596084));
#10622=CARTESIAN_POINT('Origin',(-0.330165623843516,-0.4,0.72869105993694));
#10623=CARTESIAN_POINT('',(-0.330165623843516,-0.4,0.72869105993694));
#10624=CARTESIAN_POINT('',(-0.25715157224253,-0.4,0.757544103596084));
#10625=CARTESIAN_POINT('',(-0.330165623843516,-1.,0.72869105993694));
#10626=CARTESIAN_POINT('',(-0.311912110943269,-1.,0.735904320851726));
#10627=CARTESIAN_POINT('',(-0.330165623843516,-0.4,0.72869105993694));
#10628=CARTESIAN_POINT('Origin',(-0.4,-0.4,0.692820323027551));
#10629=CARTESIAN_POINT('',(-0.4,-0.4,0.692820323027551));
#10630=CARTESIAN_POINT('',(-0.330165623843516,-0.4,0.72869105993694));
#10631=CARTESIAN_POINT('',(-0.4,-1.,0.692820323027551));
#10632=CARTESIAN_POINT('',(-0.382541405960879,-1.,0.701788007254898));
#10633=CARTESIAN_POINT('',(-0.4,-0.4,0.692820323027551));
#10634=CARTESIAN_POINT('Origin',(-0.465982157494242,-0.4,0.650277347673292));
#10635=CARTESIAN_POINT('',(-0.465982157494242,-0.4,0.650277347673292));
#10636=CARTESIAN_POINT('',(-0.4,-0.4,0.692820323027551));
#10637=CARTESIAN_POINT('',(-0.465982157494242,-1.,0.650277347673292));
#10638=CARTESIAN_POINT('',(-0.449486618120682,-1.,0.660913091511857));
#10639=CARTESIAN_POINT('',(-0.465982157494242,-0.4,0.650277347673292));
#10640=CARTESIAN_POINT('Origin',(-0.527476652080055,-0.4,0.601471845983182));
#10641=CARTESIAN_POINT('',(-0.527476652080055,-0.4,0.601471845983182));
#10642=CARTESIAN_POINT('',(-0.465982157494242,-0.4,0.650277347673292));
#10643=CARTESIAN_POINT('',(-0.527476652080055,-1.,0.601471845983182));
#10644=CARTESIAN_POINT('',(-0.512103028433602,-1.,0.613673221405709));
#10645=CARTESIAN_POINT('',(-0.527476652080055,-0.4,0.601471845983182));
#10646=CARTESIAN_POINT('Origin',(-0.583891258158269,-0.4,0.546873841618297));
#10647=CARTESIAN_POINT('',(-0.583891258158269,-0.4,0.546873841618297));
#10648=CARTESIAN_POINT('',(-0.527476652080055,-0.4,0.601471845983182));
#10649=CARTESIAN_POINT('',(-0.583891258158269,-1.,0.546873841618297));
#10650=CARTESIAN_POINT('',(-0.569787606638716,-1.,0.560523342709518));
#10651=CARTESIAN_POINT('',(-0.583891258158269,-0.4,0.546873841618297));
#10652=CARTESIAN_POINT('Origin',(-0.634682672232988,-0.4,0.487009143206976));
#10653=CARTESIAN_POINT('',(-0.634682672232988,-0.4,0.487009143206976));
#10654=CARTESIAN_POINT('',(-0.583891258158269,-0.4,0.546873841618297));
#10655=CARTESIAN_POINT('',(-0.634682672232988,-1.,0.487009143206976));
#10656=CARTESIAN_POINT('',(-0.621984818714309,-1.,0.501975317809806));
#10657=CARTESIAN_POINT('',(-0.634682672232988,-0.4,0.487009143206976));
#10658=CARTESIAN_POINT('Origin',(-1.08689407619899,-0.4,0.834003157741947));
#10659=CARTESIAN_POINT('',(-0.634682672232988,-0.4,0.487009143206976));
#10660=CARTESIAN_POINT('',(-0.543447038099496,-1.,0.417001578870973));
#10661=CARTESIAN_POINT('Origin',(-0.527275906502258,-0.4,0.913268659668846));
#10662=CARTESIAN_POINT('Origin',(0.,-1.,0.));
#10663=CARTESIAN_POINT('Origin',(0.,-1.,0.));
#10664=CARTESIAN_POINT('Origin',(0.,-1.,0.));
#10665=CARTESIAN_POINT('Origin',(0.,-1.,0.));
#10666=CARTESIAN_POINT('Origin',(0.,-1.,0.));
#10667=CARTESIAN_POINT('Origin',(0.,-1.,0.));
#10668=CARTESIAN_POINT('Origin',(0.,-1.,0.));
#10669=CARTESIAN_POINT('Origin',(0.,-1.,0.));
#10670=CARTESIAN_POINT('Origin',(0.,-1.,0.));
#10671=CARTESIAN_POINT('Origin',(0.,-1.,0.));
#10672=CARTESIAN_POINT('Origin',(0.,-1.,0.));
#10673=CARTESIAN_POINT('Origin',(0.,-1.,0.));
#10674=CARTESIAN_POINT('Origin',(0.,-1.,0.));
#10675=CARTESIAN_POINT('Origin',(0.,-1.,0.));
#10676=CARTESIAN_POINT('Origin',(0.,-1.,0.));
#10677=CARTESIAN_POINT('Origin',(0.,-1.,0.));
#10678=CARTESIAN_POINT('Origin',(0.,-1.,0.));
#10679=CARTESIAN_POINT('',(1.26571495954046,-1.,0.524276302340173));
#10680=CARTESIAN_POINT('Origin',(0.,-1.,0.));
#10681=CARTESIAN_POINT('',(0.739103626009029,-1.,0.306146745892072));
#10682=CARTESIAN_POINT('',(0.632857479770231,-1.,0.262138151170086));
#10683=CARTESIAN_POINT('',(0.765552268585767,-1.,0.23222774180357));
#10684=CARTESIAN_POINT('',(0.745715786653214,-1.,0.287666994869947));
#10685=CARTESIAN_POINT('',(0.784628224322584,-1.,0.156072257612903));
#10686=CARTESIAN_POINT('',(0.770321257519971,-1.,0.213188870755903));
#10687=CARTESIAN_POINT('',(0.796147781337758,-1.,0.0784137122636485));
#10688=CARTESIAN_POINT('',(0.787508113576378,-1.,0.136657621275589));
#10689=CARTESIAN_POINT('',(0.8,-1.,0.));
#10690=CARTESIAN_POINT('',(0.797110836003318,-1.,0.0588102841977364));
#10691=CARTESIAN_POINT('',(0.796147781337758,-1.,-0.0784137122636485));
#10692=CARTESIAN_POINT('',(0.799036945334439,-1.,-0.0196034280659122));
#10693=CARTESIAN_POINT('',(0.784628224322584,-1.,-0.156072257612903));
#10694=CARTESIAN_POINT('',(0.793267892083964,-1.,-0.0978283486009621));
#10695=CARTESIAN_POINT('',(0.765552268585767,-1.,-0.23222774180357));
#10696=CARTESIAN_POINT('',(0.77985923538838,-1.,-0.17511112866057));
#10697=CARTESIAN_POINT('',(0.739103626009029,-1.,-0.306146745892072));
#10698=CARTESIAN_POINT('',(0.758940107941583,-1.,-0.250707492825696));
#10699=CARTESIAN_POINT('',(1.26571495954046,-1.,-0.524276302340173));
#10700=CARTESIAN_POINT('',(0.369551813004515,-1.,-0.153073372946036));
#10701=CARTESIAN_POINT('',(-0.17882088334147,-1.,-1.35827946008212));
#10702=CARTESIAN_POINT('Origin',(0.,-1.,0.));
#10703=CARTESIAN_POINT('',(-0.104420953776041,-1.,-0.793155889099048));
#10704=CARTESIAN_POINT('',(-0.0894104416707352,-1.,-0.67913973004106));
#10705=CARTESIAN_POINT('',(-0.181661010427498,-1.,-0.779101583421867));
#10706=CARTESIAN_POINT('',(-0.123730967938905,-1.,-0.789642312679753));
#10707=CARTESIAN_POINT('',(-0.257151572242529,-1.,-0.757544103596085));
#10708=CARTESIAN_POINT('',(-0.200533650881256,-1.,-0.773712213465422));
#10709=CARTESIAN_POINT('',(-0.330165623843516,-1.,-0.728691059936941));
#10710=CARTESIAN_POINT('',(-0.275405085142776,-1.,-0.750330842681299));
#10711=CARTESIAN_POINT('',(-0.4,-1.,-0.692820323027551));
#10712=CARTESIAN_POINT('',(-0.347624217882637,-1.,-0.719723375709593));
#10713=CARTESIAN_POINT('',(-0.465982157494242,-1.,-0.650277347673292));
#10714=CARTESIAN_POINT('',(-0.41649553937356,-1.,-0.682184579188986));
#10715=CARTESIAN_POINT('',(-0.527476652080055,-1.,-0.601471845983182));
#10716=CARTESIAN_POINT('',(-0.481355781140695,-1.,-0.638075972250765));
#10717=CARTESIAN_POINT('',(-0.583891258158268,-1.,-0.546873841618297));
#10718=CARTESIAN_POINT('',(-0.541580303599609,-1.,-0.587822344891961));
#10719=CARTESIAN_POINT('',(-0.634682672232988,-1.,-0.487009143206977));
#10720=CARTESIAN_POINT('',(-0.596589111676948,-1.,-0.531907667015467));
#10721=CARTESIAN_POINT('',(-1.08689407619899,-1.,-0.834003157741947));
#10722=CARTESIAN_POINT('',(-0.317341336116494,-1.,-0.243504571603488));
#10723=CARTESIAN_POINT('',(-1.37,-1.,-1.67776611483187E-16));
#10724=CARTESIAN_POINT('Origin',(0.,-1.,0.));
#10725=CARTESIAN_POINT('Origin',(0.,-1.,0.));
#10726=CARTESIAN_POINT('Origin',(-0.311094480357091,-0.4,-1.33421146160995));
#10727=CARTESIAN_POINT('',(-0.17882088334147,-0.4,-1.35827946008212));
#10728=CARTESIAN_POINT('',(-0.311094480357091,-0.4,-1.33421146160995));
#10729=CARTESIAN_POINT('',(-0.17882088334147,-0.4,-1.35827946008212));
#10730=CARTESIAN_POINT('',(-0.17882088334147,-0.4,-1.35827946008212));
#10731=CARTESIAN_POINT('',(-0.311094480357091,-1.,-1.33421146160995));
#10732=CARTESIAN_POINT('',(-0.278026081103185,-1.,-1.34022846122799));
#10733=CARTESIAN_POINT('',(-0.311094480357091,-0.4,-1.33421146160995));
#10734=CARTESIAN_POINT('Origin',(-0.440372067465331,-0.4,-1.29729427740829));
#10735=CARTESIAN_POINT('',(-0.440372067465331,-0.4,-1.29729427740829));
#10736=CARTESIAN_POINT('',(-0.311094480357091,-0.4,-1.33421146160995));
#10737=CARTESIAN_POINT('',(-0.440372067465331,-1.,-1.29729427740829));
#10738=CARTESIAN_POINT('',(-0.408052670688271,-1.,-1.30652357345871));
#10739=CARTESIAN_POINT('',(-0.440372067465331,-0.4,-1.29729427740829));
#10740=CARTESIAN_POINT('Origin',(-0.565408630832021,-0.4,-1.24788344014201));
#10741=CARTESIAN_POINT('',(-0.565408630832021,-0.4,-1.24788344014201));
#10742=CARTESIAN_POINT('',(-0.440372067465331,-0.4,-1.29729427740829));
#10743=CARTESIAN_POINT('',(-0.565408630832021,-1.,-1.24788344014201));
#10744=CARTESIAN_POINT('',(-0.534149489990348,-1.,-1.26023614945858));
#10745=CARTESIAN_POINT('',(-0.565408630832021,-0.4,-1.24788344014201));
#10746=CARTESIAN_POINT('Origin',(-0.685,-0.4,-1.18645480318468));
#10747=CARTESIAN_POINT('',(-0.685,-0.4,-1.18645480318468));
#10748=CARTESIAN_POINT('',(-0.565408630832021,-0.4,-1.24788344014201));
#10749=CARTESIAN_POINT('',(-0.685,-1.,-1.18645480318468));
#10750=CARTESIAN_POINT('',(-0.655102157708006,-1.,-1.20181196242401));
#10751=CARTESIAN_POINT('',(-0.685,-0.4,-1.18645480318468));
#10752=CARTESIAN_POINT('Origin',(-0.797994444708889,-0.4,-1.11359995789051));
#10753=CARTESIAN_POINT('',(-0.797994444708889,-0.4,-1.11359995789051));
#10754=CARTESIAN_POINT('',(-0.685,-0.4,-1.18645480318468));
#10755=CARTESIAN_POINT('',(-0.797994444708889,-1.,-1.11359995789051));
#10756=CARTESIAN_POINT('',(-0.769745833531665,-1.,-1.13181366921406));
#10757=CARTESIAN_POINT('',(-0.797994444708889,-0.4,-1.11359995789051));
#10758=CARTESIAN_POINT('Origin',(-0.903303766687094,-0.4,-1.0300205362462));
#10759=CARTESIAN_POINT('',(-0.903303766687094,-0.4,-1.0300205362462));
#10760=CARTESIAN_POINT('',(-0.797994444708889,-0.4,-1.11359995789051));
#10761=CARTESIAN_POINT('',(-0.903303766687094,-1.,-1.0300205362462));
#10762=CARTESIAN_POINT('',(-0.876976436192543,-1.,-1.05091539165728));
#10763=CARTESIAN_POINT('',(-0.903303766687094,-0.4,-1.0300205362462));
#10764=CARTESIAN_POINT('Origin',(-0.999913779596035,-0.4,-0.936521453771334));
#10765=CARTESIAN_POINT('',(-0.999913779596035,-0.4,-0.936521453771334));
#10766=CARTESIAN_POINT('',(-0.903303766687094,-0.4,-1.0300205362462));
#10767=CARTESIAN_POINT('',(-0.999913779596034,-1.,-0.936521453771334));
#10768=CARTESIAN_POINT('',(-0.9757612763688,-1.,-0.95989622439005));
#10769=CARTESIAN_POINT('',(-0.999913779596035,-0.4,-0.936521453771334));
#10770=CARTESIAN_POINT('Origin',(-1.08689407619899,-0.4,-0.834003157741947));
#10771=CARTESIAN_POINT('',(-1.08689407619899,-0.4,-0.834003157741947));
#10772=CARTESIAN_POINT('',(-0.999913779596035,-0.4,-0.936521453771334));
#10773=CARTESIAN_POINT('',(-1.06514900204825,-1.,-0.859632731749293));
#10774=CARTESIAN_POINT('',(-1.08689407619899,-0.4,-0.834003157741947));
#10775=CARTESIAN_POINT('Origin',(-0.634682672232988,-0.4,-0.487009143206977));
#10776=CARTESIAN_POINT('',(-0.634682672232988,-0.4,-0.487009143206977));
#10777=CARTESIAN_POINT('',(-1.08689407619899,-0.4,-0.834003157741947));
#10778=CARTESIAN_POINT('',(-0.634682672232988,-0.4,-0.487009143206977));
#10779=CARTESIAN_POINT('Origin',(-0.583891258158268,-0.4,-0.546873841618297));
#10780=CARTESIAN_POINT('',(-0.583891258158268,-0.4,-0.546873841618297));
#10781=CARTESIAN_POINT('',(-0.634682672232988,-0.4,-0.487009143206977));
#10782=CARTESIAN_POINT('',(-0.583891258158268,-0.4,-0.546873841618297));
#10783=CARTESIAN_POINT('Origin',(-0.527476652080055,-0.4,-0.601471845983182));
#10784=CARTESIAN_POINT('',(-0.527476652080055,-0.4,-0.601471845983182));
#10785=CARTESIAN_POINT('',(-0.583891258158268,-0.4,-0.546873841618297));
#10786=CARTESIAN_POINT('',(-0.527476652080055,-0.4,-0.601471845983182));
#10787=CARTESIAN_POINT('Origin',(-0.465982157494242,-0.4,-0.650277347673292));
#10788=CARTESIAN_POINT('',(-0.465982157494242,-0.4,-0.650277347673292));
#10789=CARTESIAN_POINT('',(-0.527476652080055,-0.4,-0.601471845983182));
#10790=CARTESIAN_POINT('',(-0.465982157494242,-0.4,-0.650277347673292));
#10791=CARTESIAN_POINT('Origin',(-0.4,-0.4,-0.692820323027551));
#10792=CARTESIAN_POINT('',(-0.4,-0.4,-0.692820323027551));
#10793=CARTESIAN_POINT('',(-0.465982157494242,-0.4,-0.650277347673292));
#10794=CARTESIAN_POINT('',(-0.4,-0.4,-0.692820323027551));
#10795=CARTESIAN_POINT('Origin',(-0.330165623843516,-0.4,-0.728691059936941));
#10796=CARTESIAN_POINT('',(-0.330165623843516,-0.4,-0.728691059936941));
#10797=CARTESIAN_POINT('',(-0.4,-0.4,-0.692820323027551));
#10798=CARTESIAN_POINT('',(-0.330165623843516,-0.4,-0.728691059936941));
#10799=CARTESIAN_POINT('Origin',(-0.257151572242529,-0.4,-0.757544103596085));
#10800=CARTESIAN_POINT('',(-0.257151572242529,-0.4,-0.757544103596085));
#10801=CARTESIAN_POINT('',(-0.330165623843516,-0.4,-0.728691059936941));
#10802=CARTESIAN_POINT('',(-0.257151572242529,-0.4,-0.757544103596085));
#10803=CARTESIAN_POINT('Origin',(-0.181661010427498,-0.4,-0.779101583421867));
#10804=CARTESIAN_POINT('',(-0.181661010427498,-0.4,-0.779101583421867));
#10805=CARTESIAN_POINT('',(-0.257151572242529,-0.4,-0.757544103596085));
#10806=CARTESIAN_POINT('',(-0.181661010427498,-0.4,-0.779101583421867));
#10807=CARTESIAN_POINT('Origin',(-0.104420953776041,-0.4,-0.793155889099048));
#10808=CARTESIAN_POINT('',(-0.104420953776041,-0.4,-0.793155889099048));
#10809=CARTESIAN_POINT('',(-0.181661010427498,-0.4,-0.779101583421867));
#10810=CARTESIAN_POINT('',(-0.104420953776041,-0.4,-0.793155889099048));
#10811=CARTESIAN_POINT('Origin',(-0.17882088334147,-0.4,-1.35827946008212));
#10812=CARTESIAN_POINT('',(-0.104420953776041,-0.4,-0.793155889099048));
#10813=CARTESIAN_POINT('Origin',(-0.527275906502257,-0.4,-0.913268659668847));
#10814=CARTESIAN_POINT('Origin',(0.,-1.,0.));
#10815=CARTESIAN_POINT('Origin',(0.,-1.,0.));
#10816=CARTESIAN_POINT('Origin',(0.,-1.,0.));
#10817=CARTESIAN_POINT('Origin',(0.,-1.,0.));
#10818=CARTESIAN_POINT('Origin',(0.,-1.,0.));
#10819=CARTESIAN_POINT('Origin',(0.,-1.,0.));
#10820=CARTESIAN_POINT('Origin',(0.,-1.,0.));
#10821=CARTESIAN_POINT('Origin',(0.,-1.,0.));
#10822=CARTESIAN_POINT('Origin',(0.,-1.,0.));
#10823=CARTESIAN_POINT('Origin',(0.,-1.,0.));
#10824=CARTESIAN_POINT('Origin',(0.,-1.,0.));
#10825=CARTESIAN_POINT('Origin',(0.,-1.,0.));
#10826=CARTESIAN_POINT('Origin',(0.,-1.,0.));
#10827=CARTESIAN_POINT('Origin',(0.,-1.,0.));
#10828=CARTESIAN_POINT('Origin',(0.,-1.,0.));
#10829=CARTESIAN_POINT('Origin',(0.,-1.,0.));
#10830=CARTESIAN_POINT('Origin',(1.31100825995313,-0.4,0.397690007838613));
#10831=CARTESIAN_POINT('',(1.26571495954046,-0.4,0.524276302340173));
#10832=CARTESIAN_POINT('',(1.31100825995313,-0.4,0.397690007838613));
#10833=CARTESIAN_POINT('',(1.26571495954046,-0.4,0.524276302340173));
#10834=CARTESIAN_POINT('',(1.26571495954046,-0.4,0.524276302340173));
#10835=CARTESIAN_POINT('',(1.31100825995313,-1.,0.397690007838613));
#10836=CARTESIAN_POINT('',(1.29968493484996,-1.,0.429336581464004));
#10837=CARTESIAN_POINT('',(1.31100825995313,-0.4,0.397690007838613));
#10838=CARTESIAN_POINT('Origin',(1.34367583415243,-0.4,0.267273741162096));
#10839=CARTESIAN_POINT('',(1.34367583415243,-0.4,0.267273741162096));
#10840=CARTESIAN_POINT('',(1.31100825995313,-0.4,0.397690007838613));
#10841=CARTESIAN_POINT('',(1.34367583415243,-1.,0.267273741162096));
#10842=CARTESIAN_POINT('',(1.3355089406026,-1.,0.299877807831226));
#10843=CARTESIAN_POINT('',(1.34367583415243,-0.4,0.267273741162096));
#10844=CARTESIAN_POINT('Origin',(1.36340307554091,-0.4,0.134283482251498));
#10845=CARTESIAN_POINT('',(1.36340307554091,-0.4,0.134283482251498));
#10846=CARTESIAN_POINT('',(1.34367583415243,-0.4,0.267273741162096));
#10847=CARTESIAN_POINT('',(1.36340307554091,-1.,0.134283482251498));
#10848=CARTESIAN_POINT('',(1.35847126519379,-1.,0.167531046979148));
#10849=CARTESIAN_POINT('',(1.36340307554091,-0.4,0.134283482251498));
#10850=CARTESIAN_POINT('Origin',(1.37,-0.4,0.));
#10851=CARTESIAN_POINT('',(1.37,-0.4,0.));
#10852=CARTESIAN_POINT('',(1.36340307554091,-0.4,0.134283482251498));
#10853=CARTESIAN_POINT('',(1.37,-1.,0.));
#10854=CARTESIAN_POINT('',(1.36835076888523,-1.,0.0335708705628731));
#10855=CARTESIAN_POINT('',(1.37,-0.4,0.));
#10856=CARTESIAN_POINT('Origin',(1.36340307554091,-0.4,-0.134283482251498));
#10857=CARTESIAN_POINT('',(1.36340307554091,-0.4,-0.134283482251498));
#10858=CARTESIAN_POINT('',(1.37,-0.4,0.));
#10859=CARTESIAN_POINT('',(1.36340307554091,-1.,-0.134283482251498));
#10860=CARTESIAN_POINT('',(1.36505230665568,-1.,-0.100712611688622));
#10861=CARTESIAN_POINT('',(1.36340307554091,-0.4,-0.134283482251498));
#10862=CARTESIAN_POINT('Origin',(1.34367583415243,-0.4,-0.267273741162096));
#10863=CARTESIAN_POINT('',(1.34367583415243,-0.4,-0.267273741162096));
#10864=CARTESIAN_POINT('',(1.36340307554091,-0.4,-0.134283482251498));
#10865=CARTESIAN_POINT('',(1.34367583415243,-1.,-0.267273741162096));
#10866=CARTESIAN_POINT('',(1.34860764449955,-1.,-0.234026176434447));
#10867=CARTESIAN_POINT('',(1.34367583415243,-0.4,-0.267273741162096));
#10868=CARTESIAN_POINT('Origin',(1.31100825995313,-0.4,-0.397690007838613));
#10869=CARTESIAN_POINT('',(1.31100825995313,-0.4,-0.397690007838613));
#10870=CARTESIAN_POINT('',(1.34367583415243,-0.4,-0.267273741162096));
#10871=CARTESIAN_POINT('',(1.31100825995313,-1.,-0.397690007838613));
#10872=CARTESIAN_POINT('',(1.31917515350295,-1.,-0.365085941169485));
#10873=CARTESIAN_POINT('',(1.31100825995313,-0.4,-0.397690007838613));
#10874=CARTESIAN_POINT('Origin',(1.26571495954046,-0.4,-0.524276302340173));
#10875=CARTESIAN_POINT('',(1.26571495954046,-0.4,-0.524276302340173));
#10876=CARTESIAN_POINT('',(1.31100825995313,-0.4,-0.397690007838613));
#10877=CARTESIAN_POINT('',(1.27703828464363,-1.,-0.492629728714784));
#10878=CARTESIAN_POINT('',(1.26571495954046,-0.4,-0.524276302340173));
#10879=CARTESIAN_POINT('Origin',(0.739103626009029,-0.4,-0.306146745892072));
#10880=CARTESIAN_POINT('',(0.739103626009029,-0.4,-0.306146745892072));
#10881=CARTESIAN_POINT('',(1.26571495954046,-0.4,-0.524276302340173));
#10882=CARTESIAN_POINT('',(0.739103626009029,-0.4,-0.306146745892072));
#10883=CARTESIAN_POINT('Origin',(0.765552268585767,-0.4,-0.23222774180357));
#10884=CARTESIAN_POINT('',(0.765552268585767,-0.4,-0.23222774180357));
#10885=CARTESIAN_POINT('',(0.739103626009029,-0.4,-0.306146745892072));
#10886=CARTESIAN_POINT('',(0.765552268585767,-0.4,-0.23222774180357));
#10887=CARTESIAN_POINT('Origin',(0.784628224322584,-0.4,-0.156072257612903));
#10888=CARTESIAN_POINT('',(0.784628224322584,-0.4,-0.156072257612903));
#10889=CARTESIAN_POINT('',(0.765552268585767,-0.4,-0.23222774180357));
#10890=CARTESIAN_POINT('',(0.784628224322584,-0.4,-0.156072257612903));
#10891=CARTESIAN_POINT('Origin',(0.796147781337758,-0.4,-0.0784137122636485));
#10892=CARTESIAN_POINT('',(0.796147781337758,-0.4,-0.0784137122636485));
#10893=CARTESIAN_POINT('',(0.784628224322584,-0.4,-0.156072257612903));
#10894=CARTESIAN_POINT('',(0.796147781337758,-0.4,-0.0784137122636485));
#10895=CARTESIAN_POINT('Origin',(0.8,-0.4,0.));
#10896=CARTESIAN_POINT('',(0.8,-0.4,0.));
#10897=CARTESIAN_POINT('',(0.796147781337758,-0.4,-0.0784137122636485));
#10898=CARTESIAN_POINT('',(0.8,-0.4,0.));
#10899=CARTESIAN_POINT('Origin',(0.796147781337758,-0.4,0.0784137122636485));
#10900=CARTESIAN_POINT('',(0.796147781337758,-0.4,0.0784137122636485));
#10901=CARTESIAN_POINT('',(0.8,-0.4,0.));
#10902=CARTESIAN_POINT('',(0.796147781337758,-0.4,0.0784137122636485));
#10903=CARTESIAN_POINT('Origin',(0.784628224322584,-0.4,0.156072257612903));
#10904=CARTESIAN_POINT('',(0.784628224322584,-0.4,0.156072257612903));
#10905=CARTESIAN_POINT('',(0.796147781337758,-0.4,0.0784137122636485));
#10906=CARTESIAN_POINT('',(0.784628224322584,-0.4,0.156072257612903));
#10907=CARTESIAN_POINT('Origin',(0.765552268585767,-0.4,0.23222774180357));
#10908=CARTESIAN_POINT('',(0.765552268585767,-0.4,0.23222774180357));
#10909=CARTESIAN_POINT('',(0.784628224322584,-0.4,0.156072257612903));
#10910=CARTESIAN_POINT('',(0.765552268585767,-0.4,0.23222774180357));
#10911=CARTESIAN_POINT('Origin',(0.739103626009029,-0.4,0.306146745892072));
#10912=CARTESIAN_POINT('',(0.739103626009029,-0.4,0.306146745892072));
#10913=CARTESIAN_POINT('',(0.765552268585767,-0.4,0.23222774180357));
#10914=CARTESIAN_POINT('',(0.739103626009029,-0.4,0.306146745892072));
#10915=CARTESIAN_POINT('Origin',(1.26571495954046,-0.4,0.524276302340173));
#10916=CARTESIAN_POINT('',(0.739103626009029,-0.4,0.306146745892072));
#10917=CARTESIAN_POINT('Origin',(1.05455181300451,-0.4,0.));
#10918=CARTESIAN_POINT('Origin',(0.,-1.,0.));
#10919=CARTESIAN_POINT('Origin',(0.,-1.,0.));
#10920=CARTESIAN_POINT('Origin',(0.,-1.,0.));
#10921=CARTESIAN_POINT('Origin',(0.,-1.,0.));
#10922=CARTESIAN_POINT('Origin',(0.,-1.,0.));
#10923=CARTESIAN_POINT('Origin',(0.,-1.,0.));
#10924=CARTESIAN_POINT('Origin',(0.,-1.,0.));
#10925=CARTESIAN_POINT('Origin',(0.,-1.,0.));
#10926=CARTESIAN_POINT('Origin',(0.,-1.,0.));
#10927=CARTESIAN_POINT('Origin',(0.,-1.,0.));
#10928=CARTESIAN_POINT('Origin',(0.,-1.,0.));
#10929=CARTESIAN_POINT('Origin',(0.,-1.,0.));
#10930=CARTESIAN_POINT('Origin',(0.,-1.,0.));
#10931=CARTESIAN_POINT('Origin',(0.,-1.,0.));
#10932=CARTESIAN_POINT('Origin',(0.,-1.,0.));
#10933=CARTESIAN_POINT('Origin',(0.,-1.,0.));
#10934=CARTESIAN_POINT('Origin',(0.,-1.,0.));
#10935=CARTESIAN_POINT('',(-1.37,-2.05,1.67776611483187E-16));
#10936=CARTESIAN_POINT('Origin',(0.,-2.05,0.));
#10937=CARTESIAN_POINT('',(-1.37,-1.,-1.67776611483187E-16));
#10938=CARTESIAN_POINT('Origin',(0.,-2.05,0.));
#10939=CARTESIAN_POINT('',(0.,0.,0.));
#10940=CARTESIAN_POINT('Origin',(0.,1.525,0.));
#10941=CARTESIAN_POINT('',(0.591749422187638,1.525,0.0991595751331958));
#10942=CARTESIAN_POINT('',(0.381749422187638,1.525,0.46289024472266));
#10943=CARTESIAN_POINT('Ctrl Pts',(0.591749422187639,1.525,0.0991595751331958));
#10944=CARTESIAN_POINT('Ctrl Pts',(0.591749422187639,1.55162128248078,0.0991595751331958));
#10945=CARTESIAN_POINT('Ctrl Pts',(0.590876440724725,1.5798448972882,0.104852434209432));
#10946=CARTESIAN_POINT('Ctrl Pts',(0.586484941382362,1.63150713274392,0.127139324098885));
#10947=CARTESIAN_POINT('Ctrl Pts',(0.582861172497722,1.65496807125954,0.143660692707601));
#10948=CARTESIAN_POINT('Ctrl Pts',(0.572535383770674,1.69200621178927,0.180467056616695));
#10949=CARTESIAN_POINT('Ctrl Pts',(0.565117205136936,1.70813412776081,0.203279332063799));
#10950=CARTESIAN_POINT('Ctrl Pts',(0.545350992210601,1.72963697075952,0.251539733807139));
#10951=CARTESIAN_POINT('Ctrl Pts',(0.532918292013224,1.735,0.276958441950268));
#10952=CARTESIAN_POINT('Ctrl Pts',(0.506312192528102,1.735,0.323041558049732));
#10953=CARTESIAN_POINT('Ctrl Pts',(0.490515295643458,1.72963697075952,0.346517946329861));
#10954=CARTESIAN_POINT('Ctrl Pts',(0.45860366820005,1.70813412776081,0.387766189732349));
#10955=CARTESIAN_POINT('Ctrl Pts',(0.442556747461599,1.69200621178927,0.40559665860253));
#10956=CARTESIAN_POINT('Ctrl Pts',(0.415844395658913,1.65496807125954,0.43294223590881));
#10957=CARTESIAN_POINT('Ctrl Pts',(0.403348355180798,1.63150713274392,0.44434119612471));
#10958=CARTESIAN_POINT('Ctrl Pts',(0.386243092036367,1.5798448972882,0.459287791060626));
#10959=CARTESIAN_POINT('Ctrl Pts',(0.381749422187638,1.55162128248078,0.46289024472266));
#10960=CARTESIAN_POINT('Ctrl Pts',(0.381749422187638,1.525,0.46289024472266));
#10961=CARTESIAN_POINT('Ctrl Pts',(0.381749422187638,1.525,0.46289024472266));
#10962=CARTESIAN_POINT('Ctrl Pts',(0.381749422187638,1.49837871751922,0.46289024472266));
#10963=CARTESIAN_POINT('Ctrl Pts',(0.386243092036367,1.4701551027118,0.459287791060626));
#10964=CARTESIAN_POINT('Ctrl Pts',(0.403348355180798,1.41849286725608,0.44434119612471));
#10965=CARTESIAN_POINT('Ctrl Pts',(0.415844395658914,1.39503192874046,0.43294223590881));
#10966=CARTESIAN_POINT('Ctrl Pts',(0.442556747461599,1.35799378821073,0.40559665860253));
#10967=CARTESIAN_POINT('Ctrl Pts',(0.45860366820005,1.34186587223919,0.387766189732349));
#10968=CARTESIAN_POINT('Ctrl Pts',(0.490515295643458,1.32036302924048,0.346517946329861));
#10969=CARTESIAN_POINT('Ctrl Pts',(0.506312192528102,1.315,0.323041558049732));
#10970=CARTESIAN_POINT('Ctrl Pts',(0.532918292013224,1.315,0.276958441950268));
#10971=CARTESIAN_POINT('Ctrl Pts',(0.545350992210601,1.32036302924048,0.251539733807139));
#10972=CARTESIAN_POINT('Ctrl Pts',(0.565117205136936,1.34186587223919,0.203279332063799));
#10973=CARTESIAN_POINT('Ctrl Pts',(0.572535383770674,1.35799378821073,0.180467056616695));
#10974=CARTESIAN_POINT('Ctrl Pts',(0.582861172497722,1.39503192874046,0.143660692707601));
#10975=CARTESIAN_POINT('Ctrl Pts',(0.586484941382362,1.41849286725608,0.127139324098885));
#10976=CARTESIAN_POINT('Ctrl Pts',(0.590876440724725,1.47015510271179,0.104852434209432));
#10977=CARTESIAN_POINT('Ctrl Pts',(0.591749422187638,1.49837871751922,0.0991595751331958));
#10978=CARTESIAN_POINT('Ctrl Pts',(0.591749422187638,1.525,0.0991595751331958));
#10979=CARTESIAN_POINT('',(1.06743336697656,1.525,0.85877005482555));
#10980=CARTESIAN_POINT('',(-0.105,1.525,0.181865334794732));
#10981=CARTESIAN_POINT('',(1.27743336697656,1.525,0.495039385236086));
#10982=CARTESIAN_POINT('Ctrl Pts',(1.27743336697656,1.525,0.495039385236086));
#10983=CARTESIAN_POINT('Ctrl Pts',(1.27743336697656,1.49858689919462,0.495039385236086));
#10984=CARTESIAN_POINT('Ctrl Pts',(1.27552837579046,1.47044219200607,0.500044675653854));
#10985=CARTESIAN_POINT('Ctrl Pts',(1.26746274883014,1.41871515620915,0.520149492189153));
#10986=CARTESIAN_POINT('Ctrl Pts',(1.26126362373573,1.39512919832077,0.535224213312019));
#10987=CARTESIAN_POINT('Ctrl Pts',(1.24615878616438,1.35788630799087,0.56950781678886));
#10988=CARTESIAN_POINT('Ctrl Pts',(1.23623425750631,1.34173137598416,0.591012782176279));
#10989=CARTESIAN_POINT('Ctrl Pts',(1.213004701181,1.32028707843824,0.6373310309511));
#10990=CARTESIAN_POINT('Ctrl Pts',(1.19966110223798,1.315,0.662126019059738));
#10991=CARTESIAN_POINT('Ctrl Pts',(1.17324850413138,1.315,0.707873980940262));
#10992=CARTESIAN_POINT('Ctrl Pts',(1.15844721401428,1.32028707843824,0.731827370657151));
#10993=CARTESIAN_POINT('Ctrl Pts',(1.12994921207913,1.34173137598416,0.775103880940915));
#10994=CARTESIAN_POINT('Ctrl Pts',(1.11628763007516,1.35788630799087,0.794451257573106));
#10995=CARTESIAN_POINT('Ctrl Pts',(1.09414957731662,1.39512919832077,0.824674232368354));
#10996=CARTESIAN_POINT('Ctrl Pts',(1.08419404841645,1.41871515620915,0.837580192742778));
#10997=CARTESIAN_POINT('Ctrl Pts',(1.07081558003862,1.47044219200607,0.854617638855513));
#10998=CARTESIAN_POINT('Ctrl Pts',(1.06743336697656,1.49858689919462,0.85877005482555));
#10999=CARTESIAN_POINT('Ctrl Pts',(1.06743336697656,1.525,0.85877005482555));
#11000=CARTESIAN_POINT('Ctrl Pts',(1.06743336697656,1.525,0.85877005482555));
#11001=CARTESIAN_POINT('Ctrl Pts',(1.06743336697656,1.55141310080538,0.85877005482555));
#11002=CARTESIAN_POINT('Ctrl Pts',(1.07081558003862,1.57955780799393,0.854617638855513));
#11003=CARTESIAN_POINT('Ctrl Pts',(1.08419404841645,1.63128484379085,0.837580192742778));
#11004=CARTESIAN_POINT('Ctrl Pts',(1.09414957731662,1.65487080167923,0.824674232368354));
#11005=CARTESIAN_POINT('Ctrl Pts',(1.11628763007516,1.69211369200913,0.794451257573106));
#11006=CARTESIAN_POINT('Ctrl Pts',(1.12994921207913,1.70826862401584,0.775103880940915));
#11007=CARTESIAN_POINT('Ctrl Pts',(1.15844721401428,1.72971292156176,0.731827370657151));
#11008=CARTESIAN_POINT('Ctrl Pts',(1.17324850413138,1.735,0.707873980940262));
#11009=CARTESIAN_POINT('Ctrl Pts',(1.19966110223798,1.735,0.662126019059738));
#11010=CARTESIAN_POINT('Ctrl Pts',(1.213004701181,1.72971292156176,0.6373310309511));
#11011=CARTESIAN_POINT('Ctrl Pts',(1.23623425750631,1.70826862401584,0.591012782176279));
#11012=CARTESIAN_POINT('Ctrl Pts',(1.24615878616438,1.69211369200913,0.569507816788861));
#11013=CARTESIAN_POINT('Ctrl Pts',(1.26126362373573,1.65487080167923,0.535224213312019));
#11014=CARTESIAN_POINT('Ctrl Pts',(1.26746274883014,1.63128484379085,0.520149492189153));
#11015=CARTESIAN_POINT('Ctrl Pts',(1.27552837579046,1.57955780799392,0.500044675653854));
#11016=CARTESIAN_POINT('Ctrl Pts',(1.27743336697656,1.55141310080538,0.495039385236086));
#11017=CARTESIAN_POINT('Ctrl Pts',(1.27743336697656,1.525,0.495039385236086));
#11018=CARTESIAN_POINT('Origin',(0.,0.,0.));
#11019=CARTESIAN_POINT('',(-0.3,1.,0.519615242270663));
#11020=CARTESIAN_POINT('Origin',(0.,1.,0.));
#11021=CARTESIAN_POINT('',(-0.3,2.05,0.519615242270663));
#11022=CARTESIAN_POINT('',(-0.3,0.,0.519615242270663));
#11023=CARTESIAN_POINT('Origin',(0.,2.05,0.));
#11024=CARTESIAN_POINT('Origin',(0.181661010427498,0.4,0.779101583421867));
#11025=CARTESIAN_POINT('',(0.181661010427498,0.4,0.779101583421867));
#11026=CARTESIAN_POINT('',(0.104420953776041,0.4,0.793155889099048));
#11027=CARTESIAN_POINT('',(0.181661010427498,0.4,0.779101583421867));
#11028=CARTESIAN_POINT('',(0.104420953776041,1.,0.793155889099048));
#11029=CARTESIAN_POINT('',(0.104420953776041,0.4,0.793155889099048));
#11030=CARTESIAN_POINT('',(0.181661010427498,1.,0.779101583421867));
#11031=CARTESIAN_POINT('',(0.162350996264633,1.,0.782615159841162));
#11032=CARTESIAN_POINT('',(0.181661010427498,0.4,0.779101583421867));
#11033=CARTESIAN_POINT('Origin',(0.257151572242529,0.4,0.757544103596085));
#11034=CARTESIAN_POINT('',(0.257151572242529,0.4,0.757544103596085));
#11035=CARTESIAN_POINT('',(0.257151572242529,0.4,0.757544103596085));
#11036=CARTESIAN_POINT('',(0.257151572242529,1.,0.757544103596085));
#11037=CARTESIAN_POINT('',(0.238278931788771,1.,0.76293347355253));
#11038=CARTESIAN_POINT('',(0.257151572242529,0.4,0.757544103596085));
#11039=CARTESIAN_POINT('Origin',(0.330165623843515,0.4,0.728691059936941));
#11040=CARTESIAN_POINT('',(0.330165623843515,0.4,0.728691059936941));
#11041=CARTESIAN_POINT('',(0.330165623843515,0.4,0.728691059936941));
#11042=CARTESIAN_POINT('',(0.330165623843515,1.,0.728691059936941));
#11043=CARTESIAN_POINT('',(0.311912110943269,1.,0.735904320851727));
#11044=CARTESIAN_POINT('',(0.330165623843515,0.4,0.728691059936941));
#11045=CARTESIAN_POINT('Origin',(0.4,0.4,0.692820323027551));
#11046=CARTESIAN_POINT('',(0.4,0.4,0.692820323027551));
#11047=CARTESIAN_POINT('',(0.4,0.4,0.692820323027551));
#11048=CARTESIAN_POINT('',(0.4,1.,0.692820323027551));
#11049=CARTESIAN_POINT('',(0.382541405960878,1.,0.701788007254899));
#11050=CARTESIAN_POINT('',(0.4,0.4,0.692820323027551));
#11051=CARTESIAN_POINT('Origin',(0.465982157494241,0.4,0.650277347673292));
#11052=CARTESIAN_POINT('',(0.465982157494241,0.4,0.650277347673292));
#11053=CARTESIAN_POINT('',(0.465982157494241,0.4,0.650277347673292));
#11054=CARTESIAN_POINT('',(0.465982157494241,1.,0.650277347673292));
#11055=CARTESIAN_POINT('',(0.449486618120681,1.,0.660913091511857));
#11056=CARTESIAN_POINT('',(0.465982157494241,0.4,0.650277347673292));
#11057=CARTESIAN_POINT('Origin',(0.527476652080055,0.4,0.601471845983182));
#11058=CARTESIAN_POINT('',(0.527476652080055,0.4,0.601471845983182));
#11059=CARTESIAN_POINT('',(0.527476652080055,0.4,0.601471845983182));
#11060=CARTESIAN_POINT('',(0.527476652080055,1.,0.601471845983182));
#11061=CARTESIAN_POINT('',(0.512103028433601,1.,0.61367322140571));
#11062=CARTESIAN_POINT('',(0.527476652080055,0.4,0.601471845983182));
#11063=CARTESIAN_POINT('Origin',(0.583891258158268,0.4,0.546873841618297));
#11064=CARTESIAN_POINT('',(0.583891258158268,0.4,0.546873841618297));
#11065=CARTESIAN_POINT('',(0.583891258158268,0.4,0.546873841618297));
#11066=CARTESIAN_POINT('',(0.583891258158268,1.,0.546873841618297));
#11067=CARTESIAN_POINT('',(0.569787606638715,1.,0.560523342709519));
#11068=CARTESIAN_POINT('',(0.583891258158268,0.4,0.546873841618297));
#11069=CARTESIAN_POINT('Origin',(0.634682672232988,0.4,0.487009143206977));
#11070=CARTESIAN_POINT('',(0.634682672232988,0.4,0.487009143206977));
#11071=CARTESIAN_POINT('',(0.634682672232988,0.4,0.487009143206977));
#11072=CARTESIAN_POINT('',(0.634682672232988,1.,0.487009143206977));
#11073=CARTESIAN_POINT('',(0.621984818714308,1.,0.501975317809807));
#11074=CARTESIAN_POINT('',(0.634682672232988,0.4,0.487009143206977));
#11075=CARTESIAN_POINT('Origin',(1.08689407619899,0.4,0.834003157741948));
#11076=CARTESIAN_POINT('',(1.08689407619899,0.4,0.834003157741948));
#11077=CARTESIAN_POINT('',(1.08689407619899,0.4,0.834003157741948));
#11078=CARTESIAN_POINT('',(1.08689407619899,1.,0.834003157741948));
#11079=CARTESIAN_POINT('',(0.543447038099496,1.,0.417001578870974));
#11080=CARTESIAN_POINT('',(1.08689407619899,0.4,0.834003157741948));
#11081=CARTESIAN_POINT('Origin',(0.999913779596034,0.4,0.936521453771334));
#11082=CARTESIAN_POINT('',(0.999913779596034,0.4,0.936521453771334));
#11083=CARTESIAN_POINT('',(0.999913779596034,0.4,0.936521453771334));
#11084=CARTESIAN_POINT('',(0.999913779596034,1.,0.936521453771334));
#11085=CARTESIAN_POINT('',(1.02165885374677,1.,0.910891879763987));
#11086=CARTESIAN_POINT('',(0.999913779596034,0.4,0.936521453771334));
#11087=CARTESIAN_POINT('Origin',(0.903303766687094,0.4,1.0300205362462));
#11088=CARTESIAN_POINT('',(0.903303766687094,0.4,1.0300205362462));
#11089=CARTESIAN_POINT('',(0.903303766687094,0.4,1.0300205362462));
#11090=CARTESIAN_POINT('',(0.903303766687094,1.,1.0300205362462));
#11091=CARTESIAN_POINT('',(0.927456269914329,1.,1.00664576562748));
#11092=CARTESIAN_POINT('',(0.903303766687094,0.4,1.0300205362462));
#11093=CARTESIAN_POINT('Origin',(0.797994444708888,0.4,1.11359995789051));
#11094=CARTESIAN_POINT('',(0.797994444708888,0.4,1.11359995789051));
#11095=CARTESIAN_POINT('',(0.797994444708888,0.4,1.11359995789051));
#11096=CARTESIAN_POINT('',(0.797994444708888,1.,1.11359995789051));
#11097=CARTESIAN_POINT('',(0.82432177520344,1.,1.09270510247943));
#11098=CARTESIAN_POINT('',(0.797994444708888,0.4,1.11359995789051));
#11099=CARTESIAN_POINT('Origin',(0.684999999999999,0.4,1.18645480318468));
#11100=CARTESIAN_POINT('',(0.684999999999999,0.4,1.18645480318468));
#11101=CARTESIAN_POINT('',(0.684999999999999,0.4,1.18645480318468));
#11102=CARTESIAN_POINT('',(0.684999999999999,1.,1.18645480318468));
#11103=CARTESIAN_POINT('',(0.71324861117722,1.,1.16824109186114));
#11104=CARTESIAN_POINT('',(0.684999999999999,0.4,1.18645480318468));
#11105=CARTESIAN_POINT('Origin',(0.56540863083202,0.4,1.24788344014201));
#11106=CARTESIAN_POINT('',(0.56540863083202,0.4,1.24788344014201));
#11107=CARTESIAN_POINT('',(0.56540863083202,0.4,1.24788344014201));
#11108=CARTESIAN_POINT('',(0.56540863083202,1.,1.24788344014201));
#11109=CARTESIAN_POINT('',(0.595306473124016,1.,1.23252628090268));
#11110=CARTESIAN_POINT('',(0.56540863083202,0.4,1.24788344014201));
#11111=CARTESIAN_POINT('Origin',(0.44037206746533,0.4,1.29729427740829));
#11112=CARTESIAN_POINT('',(0.44037206746533,0.4,1.29729427740829));
#11113=CARTESIAN_POINT('',(0.44037206746533,0.4,1.29729427740829));
#11114=CARTESIAN_POINT('',(0.44037206746533,1.,1.29729427740829));
#11115=CARTESIAN_POINT('',(0.471631208307002,1.,1.28494156809172));
#11116=CARTESIAN_POINT('',(0.44037206746533,0.4,1.29729427740829));
#11117=CARTESIAN_POINT('Origin',(0.311094480357091,0.4,1.33421146160995));
#11118=CARTESIAN_POINT('',(0.311094480357091,0.4,1.33421146160995));
#11119=CARTESIAN_POINT('',(0.311094480357091,0.4,1.33421146160995));
#11120=CARTESIAN_POINT('',(0.311094480357091,1.,1.33421146160995));
#11121=CARTESIAN_POINT('',(0.34341387713415,1.,1.32498216555953));
#11122=CARTESIAN_POINT('',(0.311094480357091,0.4,1.33421146160995));
#11123=CARTESIAN_POINT('Origin',(0.17882088334147,0.4,1.35827946008212));
#11124=CARTESIAN_POINT('',(0.17882088334147,0.4,1.35827946008212));
#11125=CARTESIAN_POINT('',(0.17882088334147,0.4,1.35827946008212));
#11126=CARTESIAN_POINT('',(0.17882088334147,1.,1.35827946008212));
#11127=CARTESIAN_POINT('',(0.211889282595374,1.,1.35226246046408));
#11128=CARTESIAN_POINT('',(0.17882088334147,0.4,1.35827946008212));
#11129=CARTESIAN_POINT('Origin',(0.104420953776041,0.4,0.793155889099048));
#11130=CARTESIAN_POINT('',(0.104420953776041,0.4,0.793155889099048));
#11131=CARTESIAN_POINT('',(0.0522104768880204,1.,0.396577944549524));
#11132=CARTESIAN_POINT('Origin',(0.527275906502257,0.4,0.913268659668847));
#11133=CARTESIAN_POINT('Origin',(0.,1.,0.));
#11134=CARTESIAN_POINT('Origin',(0.,1.,0.));
#11135=CARTESIAN_POINT('Origin',(0.,1.,0.));
#11136=CARTESIAN_POINT('Origin',(0.,1.,0.));
#11137=CARTESIAN_POINT('Origin',(0.,1.,0.));
#11138=CARTESIAN_POINT('Origin',(0.,1.,0.));
#11139=CARTESIAN_POINT('Origin',(0.,1.,0.));
#11140=CARTESIAN_POINT('Origin',(0.,1.,0.));
#11141=CARTESIAN_POINT('Origin',(0.,1.,0.));
#11142=CARTESIAN_POINT('Origin',(0.,1.,0.));
#11143=CARTESIAN_POINT('Origin',(0.,1.,0.));
#11144=CARTESIAN_POINT('Origin',(0.,1.,0.));
#11145=CARTESIAN_POINT('Origin',(0.,1.,0.));
#11146=CARTESIAN_POINT('',(-0.685,1.,1.18645480318468));
#11147=CARTESIAN_POINT('Origin',(0.,1.,0.));
#11148=CARTESIAN_POINT('',(-1.26571495954046,1.,0.524276302340173));
#11149=CARTESIAN_POINT('Origin',(0.,1.,0.));
#11150=CARTESIAN_POINT('',(-0.739103626009029,1.,0.306146745892072));
#11151=CARTESIAN_POINT('',(-0.632857479770231,1.,0.262138151170086));
#11152=CARTESIAN_POINT('',(-0.765552268585767,1.,0.23222774180357));
#11153=CARTESIAN_POINT('',(-0.745715786653214,1.,0.287666994869946));
#11154=CARTESIAN_POINT('',(-0.784628224322584,1.,0.156072257612902));
#11155=CARTESIAN_POINT('',(-0.770321257519971,1.,0.213188870755903));
#11156=CARTESIAN_POINT('',(-0.796147781337758,1.,0.0784137122636482));
#11157=CARTESIAN_POINT('',(-0.787508113576378,1.,0.136657621275589));
#11158=CARTESIAN_POINT('',(-0.8,1.,-2.22044604925031E-16));
#11159=CARTESIAN_POINT('',(-0.797110836003318,1.,0.0588102841977362));
#11160=CARTESIAN_POINT('',(-0.796147781337758,1.,-0.0784137122636487));
#11161=CARTESIAN_POINT('',(-0.799036945334439,1.,-0.0196034280659124));
#11162=CARTESIAN_POINT('',(-0.784628224322584,1.,-0.156072257612903));
#11163=CARTESIAN_POINT('',(-0.793267892083964,1.,-0.0978283486009623));
#11164=CARTESIAN_POINT('',(-0.765552268585767,1.,-0.23222774180357));
#11165=CARTESIAN_POINT('',(-0.77985923538838,1.,-0.17511112866057));
#11166=CARTESIAN_POINT('',(-0.739103626009029,1.,-0.306146745892072));
#11167=CARTESIAN_POINT('',(-0.758940107941583,1.,-0.250707492825696));
#11168=CARTESIAN_POINT('',(-1.26571495954046,1.,-0.524276302340173));
#11169=CARTESIAN_POINT('',(-0.369551813004515,1.,-0.153073372946036));
#11170=CARTESIAN_POINT('',(0.178820883341471,1.,-1.35827946008212));
#11171=CARTESIAN_POINT('Origin',(0.,1.,0.));
#11172=CARTESIAN_POINT('',(0.104420953776041,1.,-0.793155889099048));
#11173=CARTESIAN_POINT('',(0.0894104416707354,1.,-0.67913973004106));
#11174=CARTESIAN_POINT('',(0.181661010427499,1.,-0.779101583421867));
#11175=CARTESIAN_POINT('',(0.123730967938906,1.,-0.789642312679753));
#11176=CARTESIAN_POINT('',(0.257151572242529,1.,-0.757544103596084));
#11177=CARTESIAN_POINT('',(0.200533650881256,1.,-0.773712213465421));
#11178=CARTESIAN_POINT('',(0.330165623843516,1.,-0.728691059936941));
#11179=CARTESIAN_POINT('',(0.275405085142776,1.,-0.750330842681299));
#11180=CARTESIAN_POINT('',(0.4,1.,-0.692820323027551));
#11181=CARTESIAN_POINT('',(0.347624217882637,1.,-0.719723375709593));
#11182=CARTESIAN_POINT('',(0.465982157494242,1.,-0.650277347673292));
#11183=CARTESIAN_POINT('',(0.416495539373561,1.,-0.682184579188986));
#11184=CARTESIAN_POINT('',(0.527476652080055,1.,-0.601471845983182));
#11185=CARTESIAN_POINT('',(0.481355781140695,1.,-0.638075972250765));
#11186=CARTESIAN_POINT('',(0.583891258158269,1.,-0.546873841618297));
#11187=CARTESIAN_POINT('',(0.541580303599609,1.,-0.587822344891961));
#11188=CARTESIAN_POINT('',(0.634682672232988,1.,-0.487009143206976));
#11189=CARTESIAN_POINT('',(0.596589111676949,1.,-0.531907667015467));
#11190=CARTESIAN_POINT('',(1.08689407619899,1.,-0.834003157741947));
#11191=CARTESIAN_POINT('',(0.317341336116494,1.,-0.243504571603488));
#11192=CARTESIAN_POINT('Origin',(0.,1.,0.));
#11193=CARTESIAN_POINT('Origin',(0.,1.,0.));
#11194=CARTESIAN_POINT('Origin',(0.,1.,0.));
#11195=CARTESIAN_POINT('Origin',(0.,1.,0.));
#11196=CARTESIAN_POINT('Origin',(0.,1.,0.));
#11197=CARTESIAN_POINT('Origin',(-0.765552268585767,0.4,-0.23222774180357));
#11198=CARTESIAN_POINT('',(-0.765552268585767,0.4,-0.23222774180357));
#11199=CARTESIAN_POINT('',(-0.739103626009029,0.4,-0.306146745892072));
#11200=CARTESIAN_POINT('',(-0.765552268585767,0.4,-0.23222774180357));
#11201=CARTESIAN_POINT('',(-0.739103626009029,0.4,-0.306146745892072));
#11202=CARTESIAN_POINT('',(-0.765552268585767,0.4,-0.23222774180357));
#11203=CARTESIAN_POINT('Origin',(-0.784628224322584,0.4,-0.156072257612903));
#11204=CARTESIAN_POINT('',(-0.784628224322584,0.4,-0.156072257612903));
#11205=CARTESIAN_POINT('',(-0.784628224322584,0.4,-0.156072257612903));
#11206=CARTESIAN_POINT('',(-0.784628224322584,0.4,-0.156072257612903));
#11207=CARTESIAN_POINT('Origin',(-0.796147781337758,0.4,-0.0784137122636487));
#11208=CARTESIAN_POINT('',(-0.796147781337758,0.4,-0.0784137122636487));
#11209=CARTESIAN_POINT('',(-0.796147781337758,0.4,-0.0784137122636487));
#11210=CARTESIAN_POINT('',(-0.796147781337758,0.4,-0.0784137122636487));
#11211=CARTESIAN_POINT('Origin',(-0.8,0.4,-2.22044604925031E-16));
#11212=CARTESIAN_POINT('',(-0.8,0.4,-2.22044604925031E-16));
#11213=CARTESIAN_POINT('',(-0.8,0.4,-2.22044604925031E-16));
#11214=CARTESIAN_POINT('',(-0.8,0.4,-2.22044604925031E-16));
#11215=CARTESIAN_POINT('Origin',(-0.796147781337758,0.4,0.0784137122636482));
#11216=CARTESIAN_POINT('',(-0.796147781337758,0.4,0.0784137122636482));
#11217=CARTESIAN_POINT('',(-0.796147781337758,0.4,0.0784137122636482));
#11218=CARTESIAN_POINT('',(-0.796147781337758,0.4,0.0784137122636482));
#11219=CARTESIAN_POINT('Origin',(-0.784628224322584,0.4,0.156072257612902));
#11220=CARTESIAN_POINT('',(-0.784628224322584,0.4,0.156072257612902));
#11221=CARTESIAN_POINT('',(-0.784628224322584,0.4,0.156072257612902));
#11222=CARTESIAN_POINT('',(-0.784628224322584,0.4,0.156072257612902));
#11223=CARTESIAN_POINT('Origin',(-0.765552268585767,0.4,0.23222774180357));
#11224=CARTESIAN_POINT('',(-0.765552268585767,0.4,0.23222774180357));
#11225=CARTESIAN_POINT('',(-0.765552268585767,0.4,0.23222774180357));
#11226=CARTESIAN_POINT('',(-0.765552268585767,0.4,0.23222774180357));
#11227=CARTESIAN_POINT('Origin',(-0.739103626009029,0.4,0.306146745892072));
#11228=CARTESIAN_POINT('',(-0.739103626009029,0.4,0.306146745892072));
#11229=CARTESIAN_POINT('',(-0.739103626009029,0.4,0.306146745892072));
#11230=CARTESIAN_POINT('',(-0.739103626009029,0.4,0.306146745892072));
#11231=CARTESIAN_POINT('Origin',(-1.26571495954046,0.4,0.524276302340173));
#11232=CARTESIAN_POINT('',(-1.26571495954046,0.4,0.524276302340173));
#11233=CARTESIAN_POINT('',(-1.26571495954046,0.4,0.524276302340173));
#11234=CARTESIAN_POINT('',(-1.26571495954046,0.4,0.524276302340173));
#11235=CARTESIAN_POINT('Origin',(-1.31100825995313,0.4,0.397690007838613));
#11236=CARTESIAN_POINT('',(-1.31100825995313,0.4,0.397690007838613));
#11237=CARTESIAN_POINT('',(-1.31100825995313,0.4,0.397690007838613));
#11238=CARTESIAN_POINT('',(-1.31100825995313,1.,0.397690007838613));
#11239=CARTESIAN_POINT('',(-1.29968493484996,1.,0.429336581464004));
#11240=CARTESIAN_POINT('',(-1.31100825995313,0.4,0.397690007838613));
#11241=CARTESIAN_POINT('Origin',(-1.34367583415243,0.4,0.267273741162095));
#11242=CARTESIAN_POINT('',(-1.34367583415243,0.4,0.267273741162095));
#11243=CARTESIAN_POINT('',(-1.34367583415243,0.4,0.267273741162095));
#11244=CARTESIAN_POINT('',(-1.34367583415243,1.,0.267273741162095));
#11245=CARTESIAN_POINT('',(-1.3355089406026,1.,0.299877807831225));
#11246=CARTESIAN_POINT('',(-1.34367583415243,0.4,0.267273741162095));
#11247=CARTESIAN_POINT('Origin',(-1.36340307554091,0.4,0.134283482251498));
#11248=CARTESIAN_POINT('',(-1.36340307554091,0.4,0.134283482251498));
#11249=CARTESIAN_POINT('',(-1.36340307554091,0.4,0.134283482251498));
#11250=CARTESIAN_POINT('',(-1.36340307554091,1.,0.134283482251498));
#11251=CARTESIAN_POINT('',(-1.35847126519379,1.,0.167531046979148));
#11252=CARTESIAN_POINT('',(-1.36340307554091,0.4,0.134283482251498));
#11253=CARTESIAN_POINT('Origin',(-1.37,0.4,-3.33066907387547E-16));
#11254=CARTESIAN_POINT('',(-1.37,0.4,-3.33066907387547E-16));
#11255=CARTESIAN_POINT('',(-1.37,0.4,-3.33066907387547E-16));
#11256=CARTESIAN_POINT('',(-1.37,1.,-3.33066907387547E-16));
#11257=CARTESIAN_POINT('',(-1.36835076888523,1.,0.0335708705628729));
#11258=CARTESIAN_POINT('',(-1.37,0.4,-3.33066907387547E-16));
#11259=CARTESIAN_POINT('Origin',(-1.36340307554091,0.4,-0.134283482251498));
#11260=CARTESIAN_POINT('',(-1.36340307554091,0.4,-0.134283482251498));
#11261=CARTESIAN_POINT('',(-1.36340307554091,0.4,-0.134283482251498));
#11262=CARTESIAN_POINT('',(-1.36340307554091,1.,-0.134283482251498));
#11263=CARTESIAN_POINT('',(-1.36505230665568,1.,-0.100712611688622));
#11264=CARTESIAN_POINT('',(-1.36340307554091,0.4,-0.134283482251498));
#11265=CARTESIAN_POINT('Origin',(-1.34367583415243,0.4,-0.267273741162096));
#11266=CARTESIAN_POINT('',(-1.34367583415243,0.4,-0.267273741162096));
#11267=CARTESIAN_POINT('',(-1.34367583415243,0.4,-0.267273741162096));
#11268=CARTESIAN_POINT('',(-1.34367583415243,1.,-0.267273741162096));
#11269=CARTESIAN_POINT('',(-1.34860764449955,1.,-0.234026176434447));
#11270=CARTESIAN_POINT('',(-1.34367583415243,0.4,-0.267273741162096));
#11271=CARTESIAN_POINT('Origin',(-1.31100825995313,0.4,-0.397690007838614));
#11272=CARTESIAN_POINT('',(-1.31100825995313,0.4,-0.397690007838614));
#11273=CARTESIAN_POINT('',(-1.31100825995313,0.4,-0.397690007838614));
#11274=CARTESIAN_POINT('',(-1.31100825995313,1.,-0.397690007838614));
#11275=CARTESIAN_POINT('',(-1.31917515350295,1.,-0.365085941169485));
#11276=CARTESIAN_POINT('',(-1.31100825995313,0.4,-0.397690007838614));
#11277=CARTESIAN_POINT('Origin',(-1.26571495954046,0.4,-0.524276302340173));
#11278=CARTESIAN_POINT('',(-1.26571495954046,0.4,-0.524276302340173));
#11279=CARTESIAN_POINT('',(-1.26571495954046,0.4,-0.524276302340173));
#11280=CARTESIAN_POINT('',(-1.27703828464363,1.,-0.492629728714784));
#11281=CARTESIAN_POINT('',(-1.26571495954046,0.4,-0.524276302340173));
#11282=CARTESIAN_POINT('Origin',(-0.739103626009029,0.4,-0.306146745892072));
#11283=CARTESIAN_POINT('',(-0.739103626009029,0.4,-0.306146745892072));
#11284=CARTESIAN_POINT('Origin',(-1.05455181300451,0.4,-3.33066907387547E-16));
#11285=CARTESIAN_POINT('Origin',(0.,1.,0.));
#11286=CARTESIAN_POINT('Origin',(0.,1.,0.));
#11287=CARTESIAN_POINT('Origin',(0.,1.,0.));
#11288=CARTESIAN_POINT('Origin',(0.,1.,0.));
#11289=CARTESIAN_POINT('Origin',(0.,1.,0.));
#11290=CARTESIAN_POINT('Origin',(0.,1.,0.));
#11291=CARTESIAN_POINT('Origin',(0.,1.,0.));
#11292=CARTESIAN_POINT('Origin',(0.,1.,0.));
#11293=CARTESIAN_POINT('Origin',(0.,1.,0.));
#11294=CARTESIAN_POINT('Origin',(0.,1.,0.));
#11295=CARTESIAN_POINT('Origin',(0.,1.,0.));
#11296=CARTESIAN_POINT('Origin',(0.,1.,0.));
#11297=CARTESIAN_POINT('Origin',(0.,1.,0.));
#11298=CARTESIAN_POINT('Origin',(0.,1.,0.));
#11299=CARTESIAN_POINT('Origin',(0.,1.,0.));
#11300=CARTESIAN_POINT('Origin',(0.,1.,0.));
#11301=CARTESIAN_POINT('Origin',(0.583891258158269,0.4,-0.546873841618297));
#11302=CARTESIAN_POINT('',(0.583891258158269,0.4,-0.546873841618297));
#11303=CARTESIAN_POINT('',(0.634682672232988,0.4,-0.487009143206976));
#11304=CARTESIAN_POINT('',(0.583891258158269,0.4,-0.546873841618297));
#11305=CARTESIAN_POINT('',(0.634682672232988,0.4,-0.487009143206976));
#11306=CARTESIAN_POINT('',(0.583891258158269,0.4,-0.546873841618297));
#11307=CARTESIAN_POINT('Origin',(0.527476652080055,0.4,-0.601471845983182));
#11308=CARTESIAN_POINT('',(0.527476652080055,0.4,-0.601471845983182));
#11309=CARTESIAN_POINT('',(0.527476652080055,0.4,-0.601471845983182));
#11310=CARTESIAN_POINT('',(0.527476652080055,0.4,-0.601471845983182));
#11311=CARTESIAN_POINT('Origin',(0.465982157494242,0.4,-0.650277347673292));
#11312=CARTESIAN_POINT('',(0.465982157494242,0.4,-0.650277347673292));
#11313=CARTESIAN_POINT('',(0.465982157494242,0.4,-0.650277347673292));
#11314=CARTESIAN_POINT('',(0.465982157494242,0.4,-0.650277347673292));
#11315=CARTESIAN_POINT('Origin',(0.4,0.4,-0.692820323027551));
#11316=CARTESIAN_POINT('',(0.4,0.4,-0.692820323027551));
#11317=CARTESIAN_POINT('',(0.4,0.4,-0.692820323027551));
#11318=CARTESIAN_POINT('',(0.4,0.4,-0.692820323027551));
#11319=CARTESIAN_POINT('Origin',(0.330165623843516,0.4,-0.728691059936941));
#11320=CARTESIAN_POINT('',(0.330165623843516,0.4,-0.728691059936941));
#11321=CARTESIAN_POINT('',(0.330165623843516,0.4,-0.728691059936941));
#11322=CARTESIAN_POINT('',(0.330165623843516,0.4,-0.728691059936941));
#11323=CARTESIAN_POINT('Origin',(0.257151572242529,0.4,-0.757544103596084));
#11324=CARTESIAN_POINT('',(0.257151572242529,0.4,-0.757544103596084));
#11325=CARTESIAN_POINT('',(0.257151572242529,0.4,-0.757544103596084));
#11326=CARTESIAN_POINT('',(0.257151572242529,0.4,-0.757544103596084));
#11327=CARTESIAN_POINT('Origin',(0.181661010427499,0.4,-0.779101583421867));
#11328=CARTESIAN_POINT('',(0.181661010427499,0.4,-0.779101583421867));
#11329=CARTESIAN_POINT('',(0.181661010427499,0.4,-0.779101583421867));
#11330=CARTESIAN_POINT('',(0.181661010427499,0.4,-0.779101583421867));
#11331=CARTESIAN_POINT('Origin',(0.104420953776041,0.4,-0.793155889099048));
#11332=CARTESIAN_POINT('',(0.104420953776041,0.4,-0.793155889099048));
#11333=CARTESIAN_POINT('',(0.104420953776041,0.4,-0.793155889099048));
#11334=CARTESIAN_POINT('',(0.104420953776041,0.4,-0.793155889099048));
#11335=CARTESIAN_POINT('Origin',(0.178820883341471,0.4,-1.35827946008212));
#11336=CARTESIAN_POINT('',(0.178820883341471,0.4,-1.35827946008212));
#11337=CARTESIAN_POINT('',(0.178820883341471,0.4,-1.35827946008212));
#11338=CARTESIAN_POINT('',(0.178820883341471,0.4,-1.35827946008212));
#11339=CARTESIAN_POINT('Origin',(0.311094480357091,0.4,-1.33421146160995));
#11340=CARTESIAN_POINT('',(0.311094480357091,0.4,-1.33421146160995));
#11341=CARTESIAN_POINT('',(0.311094480357091,0.4,-1.33421146160995));
#11342=CARTESIAN_POINT('',(0.311094480357092,1.,-1.33421146160995));
#11343=CARTESIAN_POINT('',(0.278026081103186,1.,-1.34022846122799));
#11344=CARTESIAN_POINT('',(0.311094480357091,0.4,-1.33421146160995));
#11345=CARTESIAN_POINT('Origin',(0.440372067465332,0.4,-1.29729427740829));
#11346=CARTESIAN_POINT('',(0.440372067465332,0.4,-1.29729427740829));
#11347=CARTESIAN_POINT('',(0.440372067465332,0.4,-1.29729427740829));
#11348=CARTESIAN_POINT('',(0.440372067465332,1.,-1.29729427740829));
#11349=CARTESIAN_POINT('',(0.408052670688271,1.,-1.30652357345871));
#11350=CARTESIAN_POINT('',(0.440372067465332,0.4,-1.29729427740829));
#11351=CARTESIAN_POINT('Origin',(0.565408630832021,0.4,-1.24788344014201));
#11352=CARTESIAN_POINT('',(0.565408630832021,0.4,-1.24788344014201));
#11353=CARTESIAN_POINT('',(0.565408630832021,0.4,-1.24788344014201));
#11354=CARTESIAN_POINT('',(0.565408630832021,1.,-1.24788344014201));
#11355=CARTESIAN_POINT('',(0.534149489990348,1.,-1.26023614945858));
#11356=CARTESIAN_POINT('',(0.565408630832021,0.4,-1.24788344014201));
#11357=CARTESIAN_POINT('Origin',(0.685,0.4,-1.18645480318468));
#11358=CARTESIAN_POINT('',(0.685,0.4,-1.18645480318468));
#11359=CARTESIAN_POINT('',(0.685,0.4,-1.18645480318468));
#11360=CARTESIAN_POINT('',(0.685,1.,-1.18645480318468));
#11361=CARTESIAN_POINT('',(0.655102157708007,1.,-1.20181196242401));
#11362=CARTESIAN_POINT('',(0.685,0.4,-1.18645480318468));
#11363=CARTESIAN_POINT('Origin',(0.797994444708889,0.4,-1.11359995789051));
#11364=CARTESIAN_POINT('',(0.797994444708889,0.4,-1.11359995789051));
#11365=CARTESIAN_POINT('',(0.797994444708889,0.4,-1.11359995789051));
#11366=CARTESIAN_POINT('',(0.797994444708889,1.,-1.11359995789051));
#11367=CARTESIAN_POINT('',(0.769745833531666,1.,-1.13181366921406));
#11368=CARTESIAN_POINT('',(0.797994444708889,0.4,-1.11359995789051));
#11369=CARTESIAN_POINT('Origin',(0.903303766687094,0.4,-1.0300205362462));
#11370=CARTESIAN_POINT('',(0.903303766687094,0.4,-1.0300205362462));
#11371=CARTESIAN_POINT('',(0.903303766687094,0.4,-1.0300205362462));
#11372=CARTESIAN_POINT('',(0.903303766687094,1.,-1.0300205362462));
#11373=CARTESIAN_POINT('',(0.876976436192544,1.,-1.05091539165728));
#11374=CARTESIAN_POINT('',(0.903303766687094,0.4,-1.0300205362462));
#11375=CARTESIAN_POINT('Origin',(0.999913779596035,0.4,-0.936521453771333));
#11376=CARTESIAN_POINT('',(0.999913779596035,0.4,-0.936521453771333));
#11377=CARTESIAN_POINT('',(0.999913779596035,0.4,-0.936521453771333));
#11378=CARTESIAN_POINT('',(0.999913779596035,1.,-0.936521453771333));
#11379=CARTESIAN_POINT('',(0.9757612763688,1.,-0.959896224390049));
#11380=CARTESIAN_POINT('',(0.999913779596035,0.4,-0.936521453771333));
#11381=CARTESIAN_POINT('Origin',(1.08689407619899,0.4,-0.834003157741947));
#11382=CARTESIAN_POINT('',(1.08689407619899,0.4,-0.834003157741947));
#11383=CARTESIAN_POINT('',(1.08689407619899,0.4,-0.834003157741947));
#11384=CARTESIAN_POINT('',(1.06514900204825,1.,-0.859632731749293));
#11385=CARTESIAN_POINT('',(1.08689407619899,0.4,-0.834003157741947));
#11386=CARTESIAN_POINT('Origin',(0.634682672232988,0.4,-0.487009143206976));
#11387=CARTESIAN_POINT('',(0.634682672232988,0.4,-0.487009143206976));
#11388=CARTESIAN_POINT('Origin',(0.527275906502257,0.4,-0.913268659668847));
#11389=CARTESIAN_POINT('Origin',(0.,1.,0.));
#11390=CARTESIAN_POINT('Origin',(0.,1.,0.));
#11391=CARTESIAN_POINT('Origin',(0.,1.,0.));
#11392=CARTESIAN_POINT('Origin',(0.,1.,0.));
#11393=CARTESIAN_POINT('Origin',(0.,1.,0.));
#11394=CARTESIAN_POINT('Origin',(0.,1.,0.));
#11395=CARTESIAN_POINT('Origin',(0.,1.,0.));
#11396=CARTESIAN_POINT('Origin',(0.,1.,0.));
#11397=CARTESIAN_POINT('Origin',(0.,1.,0.));
#11398=CARTESIAN_POINT('Origin',(0.,1.,0.));
#11399=CARTESIAN_POINT('Origin',(0.,1.,0.));
#11400=CARTESIAN_POINT('Origin',(0.,1.,0.));
#11401=CARTESIAN_POINT('Origin',(0.,1.,0.));
#11402=CARTESIAN_POINT('Origin',(0.,1.,0.));
#11403=CARTESIAN_POINT('Origin',(0.,1.,0.));
#11404=CARTESIAN_POINT('Origin',(0.,1.,0.));
#11405=CARTESIAN_POINT('Origin',(0.,1.,0.));
#11406=CARTESIAN_POINT('',(-0.685,2.05,1.18645480318468));
#11407=CARTESIAN_POINT('Origin',(0.,2.05,0.));
#11408=CARTESIAN_POINT('',(-0.685,1.,1.18645480318468));
#11409=CARTESIAN_POINT('Origin',(0.,2.05,0.));
#11410=CARTESIAN_POINT('',(0.,0.,0.));
#11411=CARTESIAN_POINT('Origin',(0.,-0.4,0.));
#11412=CARTESIAN_POINT('',(0.0994453842185998,-0.4,0.809917659739319));
#11413=CARTESIAN_POINT('',(0.099567253562005,-0.4,0.81091020589096));
#11414=CARTESIAN_POINT('',(0.0818108902278751,-0.4,0.666296231596819));
#11415=CARTESIAN_POINT('',(0.0663886785289718,-0.4,0.813294868644317));
#11416=CARTESIAN_POINT('',(0.091181207796194,-0.4,0.810761961965568));
#11417=CARTESIAN_POINT('',(0.0332218842499737,-0.4,0.815323436684413));
#11418=CARTESIAN_POINT('',(0.0580969799592227,-0.4,0.813802010654341));
#11419=CARTESIAN_POINT('',(-4.9960036108132E-16,-0.4,0.816));
#11420=CARTESIAN_POINT('',(0.0249164131874799,-0.4,0.81549257751331));
#11421=CARTESIAN_POINT('',(-0.0332218842499747,-0.4,0.815323436684413));
#11422=CARTESIAN_POINT('',(-0.00830547106249374,-0.4,0.815830859171103));
#11423=CARTESIAN_POINT('',(-0.0663886785289729,-0.4,0.813294868644317));
#11424=CARTESIAN_POINT('',(-0.0415135828197248,-0.4,0.814816294674389));
#11425=CARTESIAN_POINT('',(-0.0994453842186008,-0.4,0.809917659739319));
#11426=CARTESIAN_POINT('',(-0.074652854951381,-0.4,0.812450566418067));
#11427=CARTESIAN_POINT('',(-0.099567253562006,-0.4,0.81091020589096));
#11428=CARTESIAN_POINT('',(-0.0497226921093004,-0.4,0.404958829869659));
#11429=CARTESIAN_POINT('',(-0.652485211708638,-0.4,0.491682873915223));
#11430=CARTESIAN_POINT('Origin',(0.,-0.4,0.));
#11431=CARTESIAN_POINT('',(-0.651686576198591,-0.4,0.491081058892071));
#11432=CARTESIAN_POINT('',(-0.536124017894748,-0.4,0.40399842504197));
#11433=CARTESIAN_POINT('',(-0.671139677749021,-0.4,0.464141716451927));
#11434=CARTESIAN_POINT('',(-0.656549851586198,-0.4,0.484346223282036));
#11435=CARTESIAN_POINT('',(-0.689479866344548,-0.4,0.43643271406427));
#11436=CARTESIAN_POINT('',(-0.675724724897902,-0.4,0.457214465855013));
#11437=CARTESIAN_POINT('',(-0.706676729488102,-0.4,0.408));
#11438=CARTESIAN_POINT('',(-0.693779082130436,-0.4,0.429324535548202));
#11439=CARTESIAN_POINT('',(-0.722701750594522,-0.4,0.378890722620142));
#11440=CARTESIAN_POINT('',(-0.710682984764707,-0.4,0.400722680655036));
#11441=CARTESIAN_POINT('',(-0.737528356277993,-0.4,0.34915315219239));
#11442=CARTESIAN_POINT('',(-0.72640840201539,-0.4,0.371456330013204));
#11443=CARTESIAN_POINT('',(-0.751131960417191,-0.4,0.318836600847247));
#11444=CARTESIAN_POINT('',(-0.740929257312793,-0.4,0.341574014356103));
#11445=CARTESIAN_POINT('',(-0.752052465270644,-0.4,0.319227331975736));
#11446=CARTESIAN_POINT('',(-0.375565980208596,-0.4,0.159418300423624));
#11447=CARTESIAN_POINT('',(-0.752052465270644,-0.4,-0.319227331975737));
#11448=CARTESIAN_POINT('Origin',(0.,-0.4,0.));
#11449=CARTESIAN_POINT('',(-0.751131960417191,-0.4,-0.318836600847248));
#11450=CARTESIAN_POINT('',(-0.617934908122623,-0.4,-0.26229780655485));
#11451=CARTESIAN_POINT('',(-0.737528356277993,-0.4,-0.34915315219239));
#11452=CARTESIAN_POINT('',(-0.747731059382392,-0.4,-0.326415738683532));
#11453=CARTESIAN_POINT('',(-0.722701750594522,-0.4,-0.378890722620143));
#11454=CARTESIAN_POINT('',(-0.733821704857125,-0.4,-0.356587544799328));
#11455=CARTESIAN_POINT('',(-0.706676729488102,-0.4,-0.408));
#11456=CARTESIAN_POINT('',(-0.718695495317917,-0.4,-0.386168041965107));
#11457=CARTESIAN_POINT('',(-0.689479866344548,-0.4,-0.43643271406427));
#11458=CARTESIAN_POINT('',(-0.702377513702213,-0.4,-0.415108178516068));
#11459=CARTESIAN_POINT('',(-0.67113967774902,-0.4,-0.464141716451927));
#11460=CARTESIAN_POINT('',(-0.684894819195665,-0.4,-0.443359964661185));
#11461=CARTESIAN_POINT('',(-0.651686576198591,-0.4,-0.491081058892072));
#11462=CARTESIAN_POINT('',(-0.666276402361412,-0.4,-0.470876552061964));
#11463=CARTESIAN_POINT('',(-0.652485211708638,-0.4,-0.491682873915224));
#11464=CARTESIAN_POINT('',(-0.325843288099295,-0.4,-0.245540529446036));
#11465=CARTESIAN_POINT('',(-0.0995672535620054,-0.4,-0.81091020589096));
#11466=CARTESIAN_POINT('Origin',(0.,-0.4,0.));
#11467=CARTESIAN_POINT('',(-0.0994453842186002,-0.4,-0.809917659739319));
#11468=CARTESIAN_POINT('',(-0.0818108902278754,-0.4,-0.666296231596819));
#11469=CARTESIAN_POINT('',(-0.0663886785289722,-0.4,-0.813294868644317));
#11470=CARTESIAN_POINT('',(-0.0911812077961943,-0.4,-0.810761961965568));
#11471=CARTESIAN_POINT('',(-0.033221884249974,-0.4,-0.815323436684413));
#11472=CARTESIAN_POINT('',(-0.0580969799592231,-0.4,-0.813802010654341));
#11473=CARTESIAN_POINT('',(2.22044604925031E-16,-0.4,-0.816));
#11474=CARTESIAN_POINT('',(-0.0249164131874803,-0.4,-0.81549257751331));
#11475=CARTESIAN_POINT('',(0.0332218842499744,-0.4,-0.815323436684413));
#11476=CARTESIAN_POINT('',(0.00830547106249352,-0.4,-0.815830859171103));
#11477=CARTESIAN_POINT('',(0.0663886785289726,-0.4,-0.813294868644317));
#11478=CARTESIAN_POINT('',(0.0415135828197244,-0.4,-0.814816294674389));
#11479=CARTESIAN_POINT('',(0.0994453842186005,-0.4,-0.809917659739319));
#11480=CARTESIAN_POINT('',(0.0746528549513807,-0.4,-0.812450566418067));
#11481=CARTESIAN_POINT('',(0.0995672535620056,-0.4,-0.81091020589096));
#11482=CARTESIAN_POINT('',(0.0497226921093002,-0.4,-0.404958829869659));
#11483=CARTESIAN_POINT('',(0.652485211708638,-0.4,-0.491682873915223));
#11484=CARTESIAN_POINT('Origin',(0.,-0.4,0.));
#11485=CARTESIAN_POINT('',(0.651686576198591,-0.4,-0.491081058892071));
#11486=CARTESIAN_POINT('',(0.536124017894748,-0.4,-0.40399842504197));
#11487=CARTESIAN_POINT('',(0.67113967774902,-0.4,-0.464141716451927));
#11488=CARTESIAN_POINT('',(0.656549851586198,-0.4,-0.484346223282036));
#11489=CARTESIAN_POINT('',(0.689479866344548,-0.4,-0.43643271406427));
#11490=CARTESIAN_POINT('',(0.675724724897902,-0.4,-0.457214465855013));
#11491=CARTESIAN_POINT('',(0.706676729488102,-0.4,-0.408));
#11492=CARTESIAN_POINT('',(0.693779082130436,-0.4,-0.429324535548202));
#11493=CARTESIAN_POINT('',(0.722701750594522,-0.4,-0.378890722620142));
#11494=CARTESIAN_POINT('',(0.710682984764707,-0.4,-0.400722680655036));
#11495=CARTESIAN_POINT('',(0.737528356277993,-0.4,-0.34915315219239));
#11496=CARTESIAN_POINT('',(0.72640840201539,-0.4,-0.371456330013204));
#11497=CARTESIAN_POINT('',(0.751131960417191,-0.4,-0.318836600847247));
#11498=CARTESIAN_POINT('',(0.740929257312793,-0.4,-0.341574014356103));
#11499=CARTESIAN_POINT('',(0.752052465270644,-0.4,-0.319227331975737));
#11500=CARTESIAN_POINT('',(0.375565980208596,-0.4,-0.159418300423624));
#11501=CARTESIAN_POINT('',(0.752052465270643,-0.4,0.319227331975737));
#11502=CARTESIAN_POINT('Origin',(0.,-0.4,0.));
#11503=CARTESIAN_POINT('',(0.751131960417191,-0.4,0.318836600847248));
#11504=CARTESIAN_POINT('',(0.617934908122623,-0.4,0.26229780655485));
#11505=CARTESIAN_POINT('',(0.737528356277993,-0.4,0.349153152192391));
#11506=CARTESIAN_POINT('',(0.747731059382392,-0.4,0.326415738683533));
#11507=CARTESIAN_POINT('',(0.722701750594521,-0.4,0.378890722620143));
#11508=CARTESIAN_POINT('',(0.733821704857125,-0.4,0.356587544799328));
#11509=CARTESIAN_POINT('',(0.706676729488102,-0.4,0.408000000000001));
#11510=CARTESIAN_POINT('',(0.718695495317916,-0.4,0.386168041965108));
#11511=CARTESIAN_POINT('',(0.689479866344547,-0.4,0.436432714064271));
#11512=CARTESIAN_POINT('',(0.702377513702213,-0.4,0.415108178516068));
#11513=CARTESIAN_POINT('',(0.67113967774902,-0.4,0.464141716451928));
#11514=CARTESIAN_POINT('',(0.684894819195665,-0.4,0.443359964661185));
#11515=CARTESIAN_POINT('',(0.65168657619859,-0.4,0.491081058892072));
#11516=CARTESIAN_POINT('',(0.666276402361412,-0.4,0.470876552061965));
#11517=CARTESIAN_POINT('',(0.652485211708638,-0.4,0.491682873915224));
#11518=CARTESIAN_POINT('',(0.325843288099295,-0.4,0.245540529446036));
#11519=CARTESIAN_POINT('Origin',(0.,-0.4,0.));
#11520=CARTESIAN_POINT('Origin',(0.,0.,0.));
#11521=CARTESIAN_POINT('',(0.752052465270644,0.4,-0.319227331975737));
#11522=CARTESIAN_POINT('',(0.752052465270644,0.,-0.319227331975737));
#11523=CARTESIAN_POINT('',(0.752052465270643,0.4,0.319227331975737));
#11524=CARTESIAN_POINT('Origin',(0.,0.4,0.));
#11525=CARTESIAN_POINT('',(0.752052465270643,0.,0.319227331975737));
#11526=CARTESIAN_POINT('Origin',(0.,0.,0.));
#11527=CARTESIAN_POINT('',(-0.099567253562006,0.4,0.81091020589096));
#11528=CARTESIAN_POINT('',(-0.099567253562006,0.,0.81091020589096));
#11529=CARTESIAN_POINT('',(-0.652485211708638,0.4,0.491682873915223));
#11530=CARTESIAN_POINT('Origin',(0.,0.4,0.));
#11531=CARTESIAN_POINT('',(-0.652485211708638,0.,0.491682873915223));
#11532=CARTESIAN_POINT('Origin',(0.,0.,0.));
#11533=CARTESIAN_POINT('',(-0.652485211708638,0.4,-0.491682873915224));
#11534=CARTESIAN_POINT('',(-0.652485211708638,0.,-0.491682873915224));
#11535=CARTESIAN_POINT('',(-0.0995672535620054,0.4,-0.81091020589096));
#11536=CARTESIAN_POINT('Origin',(0.,0.4,0.));
#11537=CARTESIAN_POINT('',(-0.0995672535620054,0.,-0.81091020589096));
#11538=CARTESIAN_POINT('Origin',(0.,0.,0.));
#11539=CARTESIAN_POINT('',(0.652485211708638,0.4,-0.491682873915223));
#11540=CARTESIAN_POINT('',(0.652485211708638,0.,-0.491682873915223));
#11541=CARTESIAN_POINT('',(0.0995672535620056,0.4,-0.81091020589096));
#11542=CARTESIAN_POINT('',(0.0995672535620056,0.,-0.81091020589096));
#11543=CARTESIAN_POINT('Origin',(0.,0.4,0.));
#11544=CARTESIAN_POINT('Origin',(0.,0.,0.));
#11545=CARTESIAN_POINT('',(-0.752052465270644,0.4,-0.319227331975737));
#11546=CARTESIAN_POINT('',(-0.752052465270644,0.,-0.319227331975737));
#11547=CARTESIAN_POINT('',(-0.752052465270644,0.4,0.319227331975736));
#11548=CARTESIAN_POINT('',(-0.752052465270644,0.,0.319227331975736));
#11549=CARTESIAN_POINT('Origin',(0.,0.4,0.));
#11550=CARTESIAN_POINT('Origin',(0.,0.,0.));
#11551=CARTESIAN_POINT('',(0.099567253562005,0.4,0.81091020589096));
#11552=CARTESIAN_POINT('',(0.099567253562005,0.,0.81091020589096));
#11553=CARTESIAN_POINT('',(0.652485211708638,0.4,0.491682873915224));
#11554=CARTESIAN_POINT('',(0.652485211708638,0.,0.491682873915224));
#11555=CARTESIAN_POINT('Origin',(0.,0.4,0.));
#11556=CARTESIAN_POINT('Origin',(0.,0.4,0.));
#11557=CARTESIAN_POINT('',(0.0994453842185998,0.4,0.809917659739319));
#11558=CARTESIAN_POINT('',(0.0818108902278751,0.4,0.666296231596819));
#11559=CARTESIAN_POINT('',(0.65168657619859,0.4,0.491081058892072));
#11560=CARTESIAN_POINT('',(0.325843288099295,0.4,0.245540529446036));
#11561=CARTESIAN_POINT('',(0.67113967774902,0.4,0.464141716451928));
#11562=CARTESIAN_POINT('',(0.666276402361412,0.4,0.470876552061965));
#11563=CARTESIAN_POINT('',(0.689479866344547,0.4,0.436432714064271));
#11564=CARTESIAN_POINT('',(0.684894819195665,0.4,0.443359964661185));
#11565=CARTESIAN_POINT('',(0.706676729488102,0.4,0.408000000000001));
#11566=CARTESIAN_POINT('',(0.702377513702213,0.4,0.415108178516068));
#11567=CARTESIAN_POINT('',(0.722701750594521,0.4,0.378890722620143));
#11568=CARTESIAN_POINT('',(0.718695495317916,0.4,0.386168041965108));
#11569=CARTESIAN_POINT('',(0.737528356277993,0.4,0.349153152192391));
#11570=CARTESIAN_POINT('',(0.733821704857125,0.4,0.356587544799328));
#11571=CARTESIAN_POINT('',(0.751131960417191,0.4,0.318836600847248));
#11572=CARTESIAN_POINT('',(0.747731059382392,0.4,0.326415738683533));
#11573=CARTESIAN_POINT('',(0.617934908122623,0.4,0.26229780655485));
#11574=CARTESIAN_POINT('',(0.751131960417191,0.4,-0.318836600847247));
#11575=CARTESIAN_POINT('',(0.375565980208596,0.4,-0.159418300423624));
#11576=CARTESIAN_POINT('',(0.737528356277993,0.4,-0.34915315219239));
#11577=CARTESIAN_POINT('',(0.740929257312793,0.4,-0.341574014356103));
#11578=CARTESIAN_POINT('',(0.722701750594522,0.4,-0.378890722620142));
#11579=CARTESIAN_POINT('',(0.72640840201539,0.4,-0.371456330013204));
#11580=CARTESIAN_POINT('',(0.706676729488102,0.4,-0.408));
#11581=CARTESIAN_POINT('',(0.710682984764707,0.4,-0.400722680655036));
#11582=CARTESIAN_POINT('',(0.689479866344548,0.4,-0.43643271406427));
#11583=CARTESIAN_POINT('',(0.693779082130436,0.4,-0.429324535548202));
#11584=CARTESIAN_POINT('',(0.67113967774902,0.4,-0.464141716451927));
#11585=CARTESIAN_POINT('',(0.675724724897902,0.4,-0.457214465855013));
#11586=CARTESIAN_POINT('',(0.651686576198591,0.4,-0.491081058892071));
#11587=CARTESIAN_POINT('',(0.656549851586198,0.4,-0.484346223282036));
#11588=CARTESIAN_POINT('',(0.536124017894748,0.4,-0.40399842504197));
#11589=CARTESIAN_POINT('',(0.0994453842186005,0.4,-0.809917659739319));
#11590=CARTESIAN_POINT('',(0.0497226921093002,0.4,-0.404958829869659));
#11591=CARTESIAN_POINT('',(0.0663886785289726,0.4,-0.813294868644317));
#11592=CARTESIAN_POINT('',(0.0746528549513807,0.4,-0.812450566418067));
#11593=CARTESIAN_POINT('',(0.0332218842499744,0.4,-0.815323436684413));
#11594=CARTESIAN_POINT('',(0.0415135828197244,0.4,-0.814816294674389));
#11595=CARTESIAN_POINT('',(2.22044604925031E-16,0.4,-0.816));
#11596=CARTESIAN_POINT('',(0.00830547106249352,0.4,-0.815830859171103));
#11597=CARTESIAN_POINT('',(-0.033221884249974,0.4,-0.815323436684413));
#11598=CARTESIAN_POINT('',(-0.0249164131874803,0.4,-0.81549257751331));
#11599=CARTESIAN_POINT('',(-0.0663886785289722,0.4,-0.813294868644317));
#11600=CARTESIAN_POINT('',(-0.0580969799592231,0.4,-0.813802010654341));
#11601=CARTESIAN_POINT('',(-0.0994453842186002,0.4,-0.809917659739319));
#11602=CARTESIAN_POINT('',(-0.0911812077961943,0.4,-0.810761961965568));
#11603=CARTESIAN_POINT('',(-0.0818108902278754,0.4,-0.666296231596819));
#11604=CARTESIAN_POINT('',(-0.651686576198591,0.4,-0.491081058892072));
#11605=CARTESIAN_POINT('',(-0.325843288099295,0.4,-0.245540529446036));
#11606=CARTESIAN_POINT('',(-0.67113967774902,0.4,-0.464141716451927));
#11607=CARTESIAN_POINT('',(-0.666276402361412,0.4,-0.470876552061964));
#11608=CARTESIAN_POINT('',(-0.689479866344548,0.4,-0.43643271406427));
#11609=CARTESIAN_POINT('',(-0.684894819195665,0.4,-0.443359964661185));
#11610=CARTESIAN_POINT('',(-0.706676729488102,0.4,-0.408));
#11611=CARTESIAN_POINT('',(-0.702377513702213,0.4,-0.415108178516068));
#11612=CARTESIAN_POINT('',(-0.722701750594522,0.4,-0.378890722620143));
#11613=CARTESIAN_POINT('',(-0.718695495317917,0.4,-0.386168041965107));
#11614=CARTESIAN_POINT('',(-0.737528356277993,0.4,-0.34915315219239));
#11615=CARTESIAN_POINT('',(-0.733821704857125,0.4,-0.356587544799328));
#11616=CARTESIAN_POINT('',(-0.751131960417191,0.4,-0.318836600847248));
#11617=CARTESIAN_POINT('',(-0.747731059382392,0.4,-0.326415738683532));
#11618=CARTESIAN_POINT('',(-0.617934908122623,0.4,-0.26229780655485));
#11619=CARTESIAN_POINT('',(-0.751131960417191,0.4,0.318836600847247));
#11620=CARTESIAN_POINT('',(-0.375565980208596,0.4,0.159418300423624));
#11621=CARTESIAN_POINT('',(-0.737528356277993,0.4,0.34915315219239));
#11622=CARTESIAN_POINT('',(-0.740929257312793,0.4,0.341574014356103));
#11623=CARTESIAN_POINT('',(-0.722701750594522,0.4,0.378890722620142));
#11624=CARTESIAN_POINT('',(-0.72640840201539,0.4,0.371456330013204));
#11625=CARTESIAN_POINT('',(-0.706676729488102,0.4,0.408));
#11626=CARTESIAN_POINT('',(-0.710682984764707,0.4,0.400722680655036));
#11627=CARTESIAN_POINT('',(-0.689479866344548,0.4,0.43643271406427));
#11628=CARTESIAN_POINT('',(-0.693779082130436,0.4,0.429324535548202));
#11629=CARTESIAN_POINT('',(-0.671139677749021,0.4,0.464141716451927));
#11630=CARTESIAN_POINT('',(-0.675724724897902,0.4,0.457214465855013));
#11631=CARTESIAN_POINT('',(-0.651686576198591,0.4,0.491081058892071));
#11632=CARTESIAN_POINT('',(-0.656549851586198,0.4,0.484346223282036));
#11633=CARTESIAN_POINT('',(-0.536124017894748,0.4,0.40399842504197));
#11634=CARTESIAN_POINT('',(-0.0994453842186008,0.4,0.809917659739319));
#11635=CARTESIAN_POINT('',(-0.0497226921093004,0.4,0.404958829869659));
#11636=CARTESIAN_POINT('',(-0.0663886785289729,0.4,0.813294868644317));
#11637=CARTESIAN_POINT('',(-0.074652854951381,0.4,0.812450566418067));
#11638=CARTESIAN_POINT('',(-0.0332218842499747,0.4,0.815323436684413));
#11639=CARTESIAN_POINT('',(-0.0415135828197248,0.4,0.814816294674389));
#11640=CARTESIAN_POINT('',(-4.9960036108132E-16,0.4,0.816));
#11641=CARTESIAN_POINT('',(-0.00830547106249374,0.4,0.815830859171103));
#11642=CARTESIAN_POINT('',(0.0332218842499737,0.4,0.815323436684413));
#11643=CARTESIAN_POINT('',(0.0249164131874799,0.4,0.81549257751331));
#11644=CARTESIAN_POINT('',(0.0663886785289718,0.4,0.813294868644317));
#11645=CARTESIAN_POINT('',(0.0580969799592227,0.4,0.813802010654341));
#11646=CARTESIAN_POINT('',(0.091181207796194,0.4,0.810761961965568));
#11647=CARTESIAN_POINT('Origin',(1.23586981624525,0.,0.5245956131097));
#11648=CARTESIAN_POINT('',(0.751131960417191,1.,0.318836600847248));
#11649=CARTESIAN_POINT('',(0.751131960417191,0.,0.318836600847248));
#11650=CARTESIAN_POINT('',(1.23586981624525,1.,0.5245956131097));
#11651=CARTESIAN_POINT('',(1.23586981624525,1.,0.5245956131097));
#11652=CARTESIAN_POINT('',(1.23586981624525,-1.,0.5245956131097));
#11653=CARTESIAN_POINT('',(1.23586981624525,0.,0.5245956131097));
#11654=CARTESIAN_POINT('',(0.751131960417191,-1.,0.318836600847248));
#11655=CARTESIAN_POINT('',(1.23586981624525,-1.,0.5245956131097));
#11656=CARTESIAN_POINT('',(0.751131960417191,0.,0.318836600847248));
#11657=CARTESIAN_POINT('Origin',(0.751131960417191,0.,0.318836600847248));
#11658=CARTESIAN_POINT('',(0.737528356277993,1.,0.349153152192391));
#11659=CARTESIAN_POINT('',(0.737528356277993,0.,0.349153152192391));
#11660=CARTESIAN_POINT('',(0.751131960417191,1.,0.318836600847248));
#11661=CARTESIAN_POINT('Origin',(0.751131960417191,0.,0.318836600847248));
#11662=CARTESIAN_POINT('',(0.737528356277993,-1.,0.349153152192391));
#11663=CARTESIAN_POINT('',(0.751131960417191,-1.,0.318836600847248));
#11664=CARTESIAN_POINT('',(0.737528356277993,0.,0.349153152192391));
#11665=CARTESIAN_POINT('Origin',(0.737528356277993,0.,0.349153152192391));
#11666=CARTESIAN_POINT('',(0.722701750594521,1.,0.378890722620143));
#11667=CARTESIAN_POINT('',(0.722701750594521,0.,0.378890722620143));
#11668=CARTESIAN_POINT('',(0.737528356277993,1.,0.349153152192391));
#11669=CARTESIAN_POINT('Origin',(0.722701750594521,0.,0.378890722620143));
#11670=CARTESIAN_POINT('',(0.706676729488102,1.,0.408000000000001));
#11671=CARTESIAN_POINT('',(0.706676729488102,0.,0.408000000000001));
#11672=CARTESIAN_POINT('',(0.722701750594521,1.,0.378890722620143));
#11673=CARTESIAN_POINT('Origin',(0.706676729488102,0.,0.408000000000001));
#11674=CARTESIAN_POINT('',(0.689479866344547,1.,0.436432714064271));
#11675=CARTESIAN_POINT('',(0.689479866344547,0.,0.436432714064271));
#11676=CARTESIAN_POINT('',(0.706676729488102,1.,0.408000000000001));
#11677=CARTESIAN_POINT('Origin',(0.689479866344547,0.,0.436432714064271));
#11678=CARTESIAN_POINT('',(0.67113967774902,1.,0.464141716451928));
#11679=CARTESIAN_POINT('',(0.67113967774902,0.,0.464141716451928));
#11680=CARTESIAN_POINT('',(0.689479866344547,1.,0.436432714064271));
#11681=CARTESIAN_POINT('Origin',(0.67113967774902,0.,0.464141716451928));
#11682=CARTESIAN_POINT('',(0.65168657619859,1.,0.491081058892072));
#11683=CARTESIAN_POINT('',(0.65168657619859,0.,0.491081058892072));
#11684=CARTESIAN_POINT('',(0.67113967774902,1.,0.464141716451928));
#11685=CARTESIAN_POINT('Origin',(0.932067487714439,-1.,0.53812941493483));
#11686=CARTESIAN_POINT('',(1.07224803578949,-1.,0.807996850083941));
#11687=CARTESIAN_POINT('',(0.65168657619859,-1.,0.491081058892072));
#11688=CARTESIAN_POINT('',(0.65168657619859,-1.,0.491081058892072));
#11689=CARTESIAN_POINT('',(0.67113967774902,-1.,0.464141716451928));
#11690=CARTESIAN_POINT('',(0.67113967774902,-1.,0.464141716451928));
#11691=CARTESIAN_POINT('',(0.689479866344547,-1.,0.436432714064271));
#11692=CARTESIAN_POINT('',(0.689479866344547,-1.,0.436432714064271));
#11693=CARTESIAN_POINT('',(0.706676729488102,-1.,0.408000000000001));
#11694=CARTESIAN_POINT('',(0.706676729488102,-1.,0.408000000000001));
#11695=CARTESIAN_POINT('',(0.722701750594521,-1.,0.378890722620143));
#11696=CARTESIAN_POINT('',(0.722701750594521,-1.,0.378890722620143));
#11697=CARTESIAN_POINT('',(0.737528356277993,-1.,0.349153152192391));
#11698=CARTESIAN_POINT('',(1.21348721953288,-1.,0.574476742810666));
#11699=CARTESIAN_POINT('',(1.21348721953288,-1.,0.574476742810666));
#11700=CARTESIAN_POINT('',(1.1890923656228,-1.,0.623405250232603));
#11701=CARTESIAN_POINT('',(1.1890923656228,-1.,0.623405250232603));
#11702=CARTESIAN_POINT('',(1.16272570712099,-1.,0.671300000000001));
#11703=CARTESIAN_POINT('',(1.16272570712099,-1.,0.671300000000001));
#11704=CARTESIAN_POINT('',(1.13443096636543,-1.,0.718081570959179));
#11705=CARTESIAN_POINT('',(1.13443096636543,-1.,0.718081570959179));
#11706=CARTESIAN_POINT('',(1.10425506292382,-1.,0.76367238787789));
#11707=CARTESIAN_POINT('',(1.10425506292382,-1.,0.76367238787789));
#11708=CARTESIAN_POINT('',(1.07224803578949,-1.,0.807996850083941));
#11709=CARTESIAN_POINT('Origin',(0.67113967774902,0.,0.464141716451928));
#11710=CARTESIAN_POINT('',(0.67113967774902,0.,0.464141716451928));
#11711=CARTESIAN_POINT('',(0.65168657619859,0.,0.491081058892072));
#11712=CARTESIAN_POINT('Origin',(0.689479866344547,0.,0.436432714064271));
#11713=CARTESIAN_POINT('',(0.689479866344547,0.,0.436432714064271));
#11714=CARTESIAN_POINT('Origin',(0.706676729488102,0.,0.408000000000001));
#11715=CARTESIAN_POINT('',(0.706676729488102,0.,0.408000000000001));
#11716=CARTESIAN_POINT('Origin',(0.722701750594521,0.,0.378890722620143));
#11717=CARTESIAN_POINT('',(0.722701750594521,0.,0.378890722620143));
#11718=CARTESIAN_POINT('Origin',(0.737528356277993,0.,0.349153152192391));
#11719=CARTESIAN_POINT('Origin',(1.21348721953288,0.,0.574476742810666));
#11720=CARTESIAN_POINT('',(1.21348721953288,1.,0.574476742810666));
#11721=CARTESIAN_POINT('',(1.21348721953288,1.,0.574476742810666));
#11722=CARTESIAN_POINT('',(1.21348721953288,0.,0.574476742810666));
#11723=CARTESIAN_POINT('Origin',(1.1890923656228,0.,0.623405250232603));
#11724=CARTESIAN_POINT('',(1.1890923656228,1.,0.623405250232603));
#11725=CARTESIAN_POINT('',(1.1890923656228,1.,0.623405250232603));
#11726=CARTESIAN_POINT('',(1.1890923656228,0.,0.623405250232603));
#11727=CARTESIAN_POINT('Origin',(1.16272570712099,0.,0.671300000000001));
#11728=CARTESIAN_POINT('',(1.16272570712099,1.,0.671300000000001));
#11729=CARTESIAN_POINT('',(1.16272570712099,1.,0.671300000000001));
#11730=CARTESIAN_POINT('',(1.16272570712099,0.,0.671300000000001));
#11731=CARTESIAN_POINT('Origin',(1.13443096636543,0.,0.718081570959179));
#11732=CARTESIAN_POINT('',(1.13443096636543,1.,0.718081570959179));
#11733=CARTESIAN_POINT('',(1.13443096636543,1.,0.718081570959179));
#11734=CARTESIAN_POINT('',(1.13443096636543,0.,0.718081570959179));
#11735=CARTESIAN_POINT('Origin',(1.10425506292382,0.,0.76367238787789));
#11736=CARTESIAN_POINT('',(1.10425506292382,1.,0.76367238787789));
#11737=CARTESIAN_POINT('',(1.10425506292382,1.,0.76367238787789));
#11738=CARTESIAN_POINT('',(1.10425506292382,0.,0.76367238787789));
#11739=CARTESIAN_POINT('Origin',(1.07224803578949,0.,0.807996850083941));
#11740=CARTESIAN_POINT('',(1.07224803578949,1.,0.807996850083941));
#11741=CARTESIAN_POINT('',(1.07224803578949,1.,0.807996850083941));
#11742=CARTESIAN_POINT('',(1.07224803578949,0.,0.807996850083941));
#11743=CARTESIAN_POINT('Origin',(0.65168657619859,0.,0.491081058892072));
#11744=CARTESIAN_POINT('',(0.65168657619859,1.,0.491081058892072));
#11745=CARTESIAN_POINT('Origin',(0.932067487714439,1.,0.53812941493483));
#11746=CARTESIAN_POINT('Origin',(-1.0722480357895,0.,0.80799685008394));
#11747=CARTESIAN_POINT('',(-0.651686576198591,1.,0.491081058892071));
#11748=CARTESIAN_POINT('',(-0.651686576198591,0.,0.491081058892071));
#11749=CARTESIAN_POINT('',(-1.0722480357895,1.,0.80799685008394));
#11750=CARTESIAN_POINT('',(-1.0722480357895,1.,0.80799685008394));
#11751=CARTESIAN_POINT('',(-1.0722480357895,-1.,0.80799685008394));
#11752=CARTESIAN_POINT('',(-1.0722480357895,0.,0.80799685008394));
#11753=CARTESIAN_POINT('',(-0.651686576198591,-1.,0.491081058892071));
#11754=CARTESIAN_POINT('',(-1.0722480357895,-1.,0.80799685008394));
#11755=CARTESIAN_POINT('',(-0.651686576198591,0.,0.491081058892071));
#11756=CARTESIAN_POINT('Origin',(-0.651686576198591,0.,0.491081058892071));
#11757=CARTESIAN_POINT('',(-0.671139677749021,1.,0.464141716451927));
#11758=CARTESIAN_POINT('',(-0.671139677749021,0.,0.464141716451927));
#11759=CARTESIAN_POINT('',(-0.651686576198591,1.,0.491081058892071));
#11760=CARTESIAN_POINT('Origin',(-0.651686576198591,0.,0.491081058892071));
#11761=CARTESIAN_POINT('',(-0.671139677749021,-1.,0.464141716451927));
#11762=CARTESIAN_POINT('',(-0.651686576198591,-1.,0.491081058892071));
#11763=CARTESIAN_POINT('',(-0.671139677749021,0.,0.464141716451927));
#11764=CARTESIAN_POINT('Origin',(-0.671139677749021,0.,0.464141716451927));
#11765=CARTESIAN_POINT('',(-0.689479866344548,1.,0.43643271406427));
#11766=CARTESIAN_POINT('',(-0.689479866344548,0.,0.43643271406427));
#11767=CARTESIAN_POINT('',(-0.671139677749021,1.,0.464141716451927));
#11768=CARTESIAN_POINT('Origin',(-0.689479866344548,0.,0.43643271406427));
#11769=CARTESIAN_POINT('',(-0.706676729488102,1.,0.408));
#11770=CARTESIAN_POINT('',(-0.706676729488102,0.,0.408));
#11771=CARTESIAN_POINT('',(-0.689479866344548,1.,0.43643271406427));
#11772=CARTESIAN_POINT('Origin',(-0.706676729488102,0.,0.408));
#11773=CARTESIAN_POINT('',(-0.722701750594522,1.,0.378890722620142));
#11774=CARTESIAN_POINT('',(-0.722701750594522,0.,0.378890722620142));
#11775=CARTESIAN_POINT('',(-0.706676729488102,1.,0.408));
#11776=CARTESIAN_POINT('Origin',(-0.722701750594522,0.,0.378890722620142));
#11777=CARTESIAN_POINT('',(-0.737528356277993,1.,0.34915315219239));
#11778=CARTESIAN_POINT('',(-0.737528356277993,0.,0.34915315219239));
#11779=CARTESIAN_POINT('',(-0.722701750594522,1.,0.378890722620142));
#11780=CARTESIAN_POINT('Origin',(-0.737528356277993,0.,0.34915315219239));
#11781=CARTESIAN_POINT('',(-0.751131960417191,1.,0.318836600847247));
#11782=CARTESIAN_POINT('',(-0.751131960417191,0.,0.318836600847247));
#11783=CARTESIAN_POINT('',(-0.737528356277993,1.,0.34915315219239));
#11784=CARTESIAN_POINT('Origin',(-0.932067487714439,-1.,0.538129414934829));
#11785=CARTESIAN_POINT('',(-1.23586981624525,-1.,0.524595613109699));
#11786=CARTESIAN_POINT('',(-0.751131960417191,-1.,0.318836600847247));
#11787=CARTESIAN_POINT('',(-0.751131960417191,-1.,0.318836600847247));
#11788=CARTESIAN_POINT('',(-0.737528356277993,-1.,0.34915315219239));
#11789=CARTESIAN_POINT('',(-0.737528356277993,-1.,0.34915315219239));
#11790=CARTESIAN_POINT('',(-0.722701750594522,-1.,0.378890722620142));
#11791=CARTESIAN_POINT('',(-0.722701750594522,-1.,0.378890722620142));
#11792=CARTESIAN_POINT('',(-0.706676729488102,-1.,0.408));
#11793=CARTESIAN_POINT('',(-0.706676729488102,-1.,0.408));
#11794=CARTESIAN_POINT('',(-0.689479866344548,-1.,0.43643271406427));
#11795=CARTESIAN_POINT('',(-0.689479866344548,-1.,0.43643271406427));
#11796=CARTESIAN_POINT('',(-0.671139677749021,-1.,0.464141716451927));
#11797=CARTESIAN_POINT('',(-1.10425506292382,-1.,0.763672387877888));
#11798=CARTESIAN_POINT('',(-1.10425506292382,-1.,0.763672387877888));
#11799=CARTESIAN_POINT('',(-1.13443096636543,-1.,0.718081570959177));
#11800=CARTESIAN_POINT('',(-1.13443096636543,-1.,0.718081570959177));
#11801=CARTESIAN_POINT('',(-1.16272570712099,-1.,0.6713));
#11802=CARTESIAN_POINT('',(-1.16272570712099,-1.,0.6713));
#11803=CARTESIAN_POINT('',(-1.1890923656228,-1.,0.623405250232602));
#11804=CARTESIAN_POINT('',(-1.1890923656228,-1.,0.623405250232602));
#11805=CARTESIAN_POINT('',(-1.21348721953288,-1.,0.574476742810665));
#11806=CARTESIAN_POINT('',(-1.21348721953288,-1.,0.574476742810665));
#11807=CARTESIAN_POINT('',(-1.23586981624525,-1.,0.524595613109699));
#11808=CARTESIAN_POINT('Origin',(-0.737528356277993,0.,0.34915315219239));
#11809=CARTESIAN_POINT('',(-0.737528356277993,0.,0.34915315219239));
#11810=CARTESIAN_POINT('',(-0.751131960417191,0.,0.318836600847247));
#11811=CARTESIAN_POINT('Origin',(-0.722701750594522,0.,0.378890722620142));
#11812=CARTESIAN_POINT('',(-0.722701750594522,0.,0.378890722620142));
#11813=CARTESIAN_POINT('Origin',(-0.706676729488102,0.,0.408));
#11814=CARTESIAN_POINT('',(-0.706676729488102,0.,0.408));
#11815=CARTESIAN_POINT('Origin',(-0.689479866344548,0.,0.43643271406427));
#11816=CARTESIAN_POINT('',(-0.689479866344548,0.,0.43643271406427));
#11817=CARTESIAN_POINT('Origin',(-0.671139677749021,0.,0.464141716451927));
#11818=CARTESIAN_POINT('Origin',(-1.10425506292382,0.,0.763672387877888));
#11819=CARTESIAN_POINT('',(-1.10425506292382,1.,0.763672387877888));
#11820=CARTESIAN_POINT('',(-1.10425506292382,1.,0.763672387877888));
#11821=CARTESIAN_POINT('',(-1.10425506292382,0.,0.763672387877888));
#11822=CARTESIAN_POINT('Origin',(-1.13443096636543,0.,0.718081570959177));
#11823=CARTESIAN_POINT('',(-1.13443096636543,1.,0.718081570959177));
#11824=CARTESIAN_POINT('',(-1.13443096636543,1.,0.718081570959177));
#11825=CARTESIAN_POINT('',(-1.13443096636543,0.,0.718081570959177));
#11826=CARTESIAN_POINT('Origin',(-1.16272570712099,0.,0.6713));
#11827=CARTESIAN_POINT('',(-1.16272570712099,1.,0.6713));
#11828=CARTESIAN_POINT('',(-1.16272570712099,1.,0.6713));
#11829=CARTESIAN_POINT('',(-1.16272570712099,0.,0.6713));
#11830=CARTESIAN_POINT('Origin',(-1.1890923656228,0.,0.623405250232602));
#11831=CARTESIAN_POINT('',(-1.1890923656228,1.,0.623405250232602));
#11832=CARTESIAN_POINT('',(-1.1890923656228,1.,0.623405250232602));
#11833=CARTESIAN_POINT('',(-1.1890923656228,0.,0.623405250232602));
#11834=CARTESIAN_POINT('Origin',(-1.21348721953288,0.,0.574476742810665));
#11835=CARTESIAN_POINT('',(-1.21348721953288,1.,0.574476742810665));
#11836=CARTESIAN_POINT('',(-1.21348721953288,1.,0.574476742810665));
#11837=CARTESIAN_POINT('',(-1.21348721953288,0.,0.574476742810665));
#11838=CARTESIAN_POINT('Origin',(-1.23586981624525,0.,0.524595613109699));
#11839=CARTESIAN_POINT('',(-1.23586981624525,1.,0.524595613109699));
#11840=CARTESIAN_POINT('',(-1.23586981624525,1.,0.524595613109699));
#11841=CARTESIAN_POINT('',(-1.23586981624525,0.,0.524595613109699));
#11842=CARTESIAN_POINT('Origin',(-0.751131960417191,0.,0.318836600847247));
#11843=CARTESIAN_POINT('',(-0.751131960417191,1.,0.318836600847247));
#11844=CARTESIAN_POINT('Origin',(-0.932067487714439,1.,0.538129414934829));
#11845=CARTESIAN_POINT('Origin',(-0.163621780455751,0.,-1.33259246319364));
#11846=CARTESIAN_POINT('',(-0.0994453842186002,1.,-0.809917659739319));
#11847=CARTESIAN_POINT('',(-0.0994453842186002,0.,-0.809917659739319));
#11848=CARTESIAN_POINT('',(-0.163621780455751,1.,-1.33259246319364));
#11849=CARTESIAN_POINT('',(-0.163621780455751,1.,-1.33259246319364));
#11850=CARTESIAN_POINT('',(-0.163621780455751,-1.,-1.33259246319364));
#11851=CARTESIAN_POINT('',(-0.163621780455751,0.,-1.33259246319364));
#11852=CARTESIAN_POINT('',(-0.0994453842186002,-1.,-0.809917659739319));
#11853=CARTESIAN_POINT('',(-0.163621780455751,-1.,-1.33259246319364));
#11854=CARTESIAN_POINT('',(-0.0994453842186002,0.,-0.809917659739319));
#11855=CARTESIAN_POINT('Origin',(-0.0994453842186002,0.,-0.809917659739319));
#11856=CARTESIAN_POINT('',(-0.0663886785289722,1.,-0.813294868644317));
#11857=CARTESIAN_POINT('',(-0.0663886785289722,0.,-0.813294868644317));
#11858=CARTESIAN_POINT('',(-0.0994453842186002,1.,-0.809917659739319));
#11859=CARTESIAN_POINT('Origin',(-0.0994453842186002,0.,-0.809917659739319));
#11860=CARTESIAN_POINT('',(-0.0663886785289722,-1.,-0.813294868644317));
#11861=CARTESIAN_POINT('',(-0.0994453842186002,-1.,-0.809917659739319));
#11862=CARTESIAN_POINT('',(-0.0663886785289722,0.,-0.813294868644317));
#11863=CARTESIAN_POINT('Origin',(-0.0663886785289722,0.,-0.813294868644317));
#11864=CARTESIAN_POINT('',(-0.033221884249974,1.,-0.815323436684413));
#11865=CARTESIAN_POINT('',(-0.033221884249974,0.,-0.815323436684413));
#11866=CARTESIAN_POINT('',(-0.0663886785289722,1.,-0.813294868644317));
#11867=CARTESIAN_POINT('Origin',(-0.033221884249974,0.,-0.815323436684413));
#11868=CARTESIAN_POINT('',(2.22044604925031E-16,1.,-0.816));
#11869=CARTESIAN_POINT('',(2.22044604925031E-16,0.,-0.816));
#11870=CARTESIAN_POINT('',(-0.033221884249974,1.,-0.815323436684413));
#11871=CARTESIAN_POINT('Origin',(2.22044604925031E-16,0.,-0.816));
#11872=CARTESIAN_POINT('',(0.0332218842499744,1.,-0.815323436684413));
#11873=CARTESIAN_POINT('',(0.0332218842499744,0.,-0.815323436684413));
#11874=CARTESIAN_POINT('',(2.22044604925031E-16,1.,-0.816));
#11875=CARTESIAN_POINT('Origin',(0.0332218842499744,0.,-0.815323436684413));
#11876=CARTESIAN_POINT('',(0.0663886785289726,1.,-0.813294868644317));
#11877=CARTESIAN_POINT('',(0.0663886785289726,0.,-0.813294868644317));
#11878=CARTESIAN_POINT('',(0.0332218842499744,1.,-0.815323436684413));
#11879=CARTESIAN_POINT('Origin',(0.0663886785289726,0.,-0.813294868644317));
#11880=CARTESIAN_POINT('',(0.0994453842186005,1.,-0.809917659739319));
#11881=CARTESIAN_POINT('',(0.0994453842186005,0.,-0.809917659739319));
#11882=CARTESIAN_POINT('',(0.0663886785289726,1.,-0.813294868644317));
#11883=CARTESIAN_POINT('Origin',(2.22044604925031E-16,-1.,-1.07625882986966));
#11884=CARTESIAN_POINT('',(0.163621780455751,-1.,-1.33259246319364));
#11885=CARTESIAN_POINT('',(0.0994453842186005,-1.,-0.809917659739319));
#11886=CARTESIAN_POINT('',(0.0994453842186005,-1.,-0.809917659739319));
#11887=CARTESIAN_POINT('',(0.0663886785289726,-1.,-0.813294868644317));
#11888=CARTESIAN_POINT('',(0.0663886785289726,-1.,-0.813294868644317));
#11889=CARTESIAN_POINT('',(0.0332218842499744,-1.,-0.815323436684413));
#11890=CARTESIAN_POINT('',(0.0332218842499744,-1.,-0.815323436684413));
#11891=CARTESIAN_POINT('',(2.22044604925031E-16,-1.,-0.816));
#11892=CARTESIAN_POINT('',(2.22044604925031E-16,-1.,-0.816));
#11893=CARTESIAN_POINT('',(-0.033221884249974,-1.,-0.815323436684413));
#11894=CARTESIAN_POINT('',(-0.033221884249974,-1.,-0.815323436684413));
#11895=CARTESIAN_POINT('',(-0.0663886785289722,-1.,-0.813294868644317));
#11896=CARTESIAN_POINT('',(-0.109232156609066,-1.,-1.33814913068855));
#11897=CARTESIAN_POINT('',(-0.109232156609066,-1.,-1.33814913068855));
#11898=CARTESIAN_POINT('',(-0.0546613992573715,-1.,-1.34148682119178));
#11899=CARTESIAN_POINT('',(-0.0546613992573715,-1.,-1.34148682119178));
#11900=CARTESIAN_POINT('',(2.22044604925031E-16,-1.,-1.3426));
#11901=CARTESIAN_POINT('',(2.22044604925031E-16,-1.,-1.3426));
#11902=CARTESIAN_POINT('',(0.054661399257372,-1.,-1.34148682119178));
#11903=CARTESIAN_POINT('',(0.054661399257372,-1.,-1.34148682119178));
#11904=CARTESIAN_POINT('',(0.109232156609067,-1.,-1.33814913068855));
#11905=CARTESIAN_POINT('',(0.109232156609067,-1.,-1.33814913068855));
#11906=CARTESIAN_POINT('',(0.163621780455751,-1.,-1.33259246319364));
#11907=CARTESIAN_POINT('Origin',(0.0663886785289726,0.,-0.813294868644317));
#11908=CARTESIAN_POINT('',(0.0663886785289726,0.,-0.813294868644317));
#11909=CARTESIAN_POINT('',(0.0994453842186005,0.,-0.809917659739319));
#11910=CARTESIAN_POINT('Origin',(0.0332218842499744,0.,-0.815323436684413));
#11911=CARTESIAN_POINT('',(0.0332218842499744,0.,-0.815323436684413));
#11912=CARTESIAN_POINT('Origin',(2.22044604925031E-16,0.,-0.816));
#11913=CARTESIAN_POINT('',(2.22044604925031E-16,0.,-0.816));
#11914=CARTESIAN_POINT('Origin',(-0.033221884249974,0.,-0.815323436684413));
#11915=CARTESIAN_POINT('',(-0.033221884249974,0.,-0.815323436684413));
#11916=CARTESIAN_POINT('Origin',(-0.0663886785289722,0.,-0.813294868644317));
#11917=CARTESIAN_POINT('Origin',(-0.109232156609066,0.,-1.33814913068855));
#11918=CARTESIAN_POINT('',(-0.109232156609066,1.,-1.33814913068855));
#11919=CARTESIAN_POINT('',(-0.109232156609066,1.,-1.33814913068855));
#11920=CARTESIAN_POINT('',(-0.109232156609066,0.,-1.33814913068855));
#11921=CARTESIAN_POINT('Origin',(-0.0546613992573715,0.,-1.34148682119178));
#11922=CARTESIAN_POINT('',(-0.0546613992573715,1.,-1.34148682119178));
#11923=CARTESIAN_POINT('',(-0.0546613992573715,1.,-1.34148682119178));
#11924=CARTESIAN_POINT('',(-0.0546613992573715,0.,-1.34148682119178));
#11925=CARTESIAN_POINT('Origin',(2.22044604925031E-16,0.,-1.3426));
#11926=CARTESIAN_POINT('',(2.22044604925031E-16,1.,-1.3426));
#11927=CARTESIAN_POINT('',(2.22044604925031E-16,1.,-1.3426));
#11928=CARTESIAN_POINT('',(2.22044604925031E-16,0.,-1.3426));
#11929=CARTESIAN_POINT('Origin',(0.054661399257372,0.,-1.34148682119178));
#11930=CARTESIAN_POINT('',(0.054661399257372,1.,-1.34148682119178));
#11931=CARTESIAN_POINT('',(0.054661399257372,1.,-1.34148682119178));
#11932=CARTESIAN_POINT('',(0.054661399257372,0.,-1.34148682119178));
#11933=CARTESIAN_POINT('Origin',(0.109232156609067,0.,-1.33814913068855));
#11934=CARTESIAN_POINT('',(0.109232156609067,1.,-1.33814913068855));
#11935=CARTESIAN_POINT('',(0.109232156609067,1.,-1.33814913068855));
#11936=CARTESIAN_POINT('',(0.109232156609067,0.,-1.33814913068855));
#11937=CARTESIAN_POINT('Origin',(0.163621780455751,0.,-1.33259246319364));
#11938=CARTESIAN_POINT('',(0.163621780455751,1.,-1.33259246319364));
#11939=CARTESIAN_POINT('',(0.163621780455751,1.,-1.33259246319364));
#11940=CARTESIAN_POINT('',(0.163621780455751,0.,-1.33259246319364));
#11941=CARTESIAN_POINT('Origin',(0.0994453842186005,0.,-0.809917659739319));
#11942=CARTESIAN_POINT('',(0.0994453842186005,1.,-0.809917659739319));
#11943=CARTESIAN_POINT('Origin',(2.22044604925031E-16,1.,-1.07625882986966));
#11944=CARTESIAN_POINT('Origin',(1.0722480357895,0.,-0.80799685008394));
#11945=CARTESIAN_POINT('',(0.651686576198591,1.,-0.491081058892071));
#11946=CARTESIAN_POINT('',(0.651686576198591,0.,-0.491081058892071));
#11947=CARTESIAN_POINT('',(1.0722480357895,1.,-0.80799685008394));
#11948=CARTESIAN_POINT('',(1.0722480357895,1.,-0.80799685008394));
#11949=CARTESIAN_POINT('',(1.0722480357895,-1.,-0.80799685008394));
#11950=CARTESIAN_POINT('',(1.0722480357895,0.,-0.80799685008394));
#11951=CARTESIAN_POINT('',(0.651686576198591,-1.,-0.491081058892071));
#11952=CARTESIAN_POINT('',(1.0722480357895,-1.,-0.80799685008394));
#11953=CARTESIAN_POINT('',(0.651686576198591,0.,-0.491081058892071));
#11954=CARTESIAN_POINT('Origin',(0.651686576198591,0.,-0.491081058892071));
#11955=CARTESIAN_POINT('',(0.67113967774902,1.,-0.464141716451927));
#11956=CARTESIAN_POINT('',(0.67113967774902,0.,-0.464141716451927));
#11957=CARTESIAN_POINT('',(0.651686576198591,1.,-0.491081058892071));
#11958=CARTESIAN_POINT('Origin',(0.651686576198591,0.,-0.491081058892071));
#11959=CARTESIAN_POINT('',(0.67113967774902,-1.,-0.464141716451927));
#11960=CARTESIAN_POINT('',(0.651686576198591,-1.,-0.491081058892071));
#11961=CARTESIAN_POINT('',(0.67113967774902,0.,-0.464141716451927));
#11962=CARTESIAN_POINT('Origin',(0.67113967774902,0.,-0.464141716451927));
#11963=CARTESIAN_POINT('',(0.689479866344548,1.,-0.43643271406427));
#11964=CARTESIAN_POINT('',(0.689479866344548,0.,-0.43643271406427));
#11965=CARTESIAN_POINT('',(0.67113967774902,1.,-0.464141716451927));
#11966=CARTESIAN_POINT('Origin',(0.689479866344548,0.,-0.43643271406427));
#11967=CARTESIAN_POINT('',(0.706676729488102,1.,-0.408));
#11968=CARTESIAN_POINT('',(0.706676729488102,0.,-0.408));
#11969=CARTESIAN_POINT('',(0.689479866344548,1.,-0.43643271406427));
#11970=CARTESIAN_POINT('Origin',(0.706676729488102,0.,-0.408));
#11971=CARTESIAN_POINT('',(0.722701750594522,1.,-0.378890722620142));
#11972=CARTESIAN_POINT('',(0.722701750594522,0.,-0.378890722620142));
#11973=CARTESIAN_POINT('',(0.706676729488102,1.,-0.408));
#11974=CARTESIAN_POINT('Origin',(0.722701750594522,0.,-0.378890722620142));
#11975=CARTESIAN_POINT('',(0.737528356277993,1.,-0.34915315219239));
#11976=CARTESIAN_POINT('',(0.737528356277993,0.,-0.34915315219239));
#11977=CARTESIAN_POINT('',(0.722701750594522,1.,-0.378890722620142));
#11978=CARTESIAN_POINT('Origin',(0.737528356277993,0.,-0.34915315219239));
#11979=CARTESIAN_POINT('',(0.751131960417191,1.,-0.318836600847247));
#11980=CARTESIAN_POINT('',(0.751131960417191,0.,-0.318836600847247));
#11981=CARTESIAN_POINT('',(0.737528356277993,1.,-0.34915315219239));
#11982=CARTESIAN_POINT('Origin',(0.932067487714439,-1.,-0.53812941493483));
#11983=CARTESIAN_POINT('',(1.23586981624525,-1.,-0.524595613109699));
#11984=CARTESIAN_POINT('',(0.751131960417191,-1.,-0.318836600847247));
#11985=CARTESIAN_POINT('',(0.751131960417191,-1.,-0.318836600847247));
#11986=CARTESIAN_POINT('',(0.737528356277993,-1.,-0.34915315219239));
#11987=CARTESIAN_POINT('',(0.737528356277993,-1.,-0.34915315219239));
#11988=CARTESIAN_POINT('',(0.722701750594522,-1.,-0.378890722620142));
#11989=CARTESIAN_POINT('',(0.722701750594522,-1.,-0.378890722620142));
#11990=CARTESIAN_POINT('',(0.706676729488102,-1.,-0.408));
#11991=CARTESIAN_POINT('',(0.706676729488102,-1.,-0.408));
#11992=CARTESIAN_POINT('',(0.689479866344548,-1.,-0.43643271406427));
#11993=CARTESIAN_POINT('',(0.689479866344548,-1.,-0.43643271406427));
#11994=CARTESIAN_POINT('',(0.67113967774902,-1.,-0.464141716451927));
#11995=CARTESIAN_POINT('',(1.10425506292382,-1.,-0.763672387877889));
#11996=CARTESIAN_POINT('',(1.10425506292382,-1.,-0.763672387877889));
#11997=CARTESIAN_POINT('',(1.13443096636543,-1.,-0.718081570959178));
#11998=CARTESIAN_POINT('',(1.13443096636543,-1.,-0.718081570959177));
#11999=CARTESIAN_POINT('',(1.16272570712099,-1.,-0.6713));
#12000=CARTESIAN_POINT('',(1.16272570712099,-1.,-0.6713));
#12001=CARTESIAN_POINT('',(1.1890923656228,-1.,-0.623405250232602));
#12002=CARTESIAN_POINT('',(1.1890923656228,-1.,-0.623405250232602));
#12003=CARTESIAN_POINT('',(1.21348721953288,-1.,-0.574476742810665));
#12004=CARTESIAN_POINT('',(1.21348721953288,-1.,-0.574476742810665));
#12005=CARTESIAN_POINT('',(1.23586981624525,-1.,-0.524595613109699));
#12006=CARTESIAN_POINT('Origin',(0.737528356277993,0.,-0.34915315219239));
#12007=CARTESIAN_POINT('',(0.737528356277993,0.,-0.34915315219239));
#12008=CARTESIAN_POINT('',(0.751131960417191,0.,-0.318836600847247));
#12009=CARTESIAN_POINT('Origin',(0.722701750594522,0.,-0.378890722620142));
#12010=CARTESIAN_POINT('',(0.722701750594522,0.,-0.378890722620142));
#12011=CARTESIAN_POINT('Origin',(0.706676729488102,0.,-0.408));
#12012=CARTESIAN_POINT('',(0.706676729488102,0.,-0.408));
#12013=CARTESIAN_POINT('Origin',(0.689479866344548,0.,-0.43643271406427));
#12014=CARTESIAN_POINT('',(0.689479866344548,0.,-0.43643271406427));
#12015=CARTESIAN_POINT('Origin',(0.67113967774902,0.,-0.464141716451927));
#12016=CARTESIAN_POINT('Origin',(1.10425506292382,0.,-0.763672387877889));
#12017=CARTESIAN_POINT('',(1.10425506292382,1.,-0.763672387877889));
#12018=CARTESIAN_POINT('',(1.10425506292382,1.,-0.763672387877889));
#12019=CARTESIAN_POINT('',(1.10425506292382,0.,-0.763672387877889));
#12020=CARTESIAN_POINT('Origin',(1.13443096636543,0.,-0.718081570959177));
#12021=CARTESIAN_POINT('',(1.13443096636543,1.,-0.718081570959178));
#12022=CARTESIAN_POINT('',(1.13443096636543,1.,-0.718081570959177));
#12023=CARTESIAN_POINT('',(1.13443096636543,0.,-0.718081570959177));
#12024=CARTESIAN_POINT('Origin',(1.16272570712099,0.,-0.6713));
#12025=CARTESIAN_POINT('',(1.16272570712099,1.,-0.6713));
#12026=CARTESIAN_POINT('',(1.16272570712099,1.,-0.6713));
#12027=CARTESIAN_POINT('',(1.16272570712099,0.,-0.6713));
#12028=CARTESIAN_POINT('Origin',(1.1890923656228,0.,-0.623405250232602));
#12029=CARTESIAN_POINT('',(1.1890923656228,1.,-0.623405250232602));
#12030=CARTESIAN_POINT('',(1.1890923656228,1.,-0.623405250232602));
#12031=CARTESIAN_POINT('',(1.1890923656228,0.,-0.623405250232602));
#12032=CARTESIAN_POINT('Origin',(1.21348721953288,0.,-0.574476742810665));
#12033=CARTESIAN_POINT('',(1.21348721953288,1.,-0.574476742810665));
#12034=CARTESIAN_POINT('',(1.21348721953288,1.,-0.574476742810665));
#12035=CARTESIAN_POINT('',(1.21348721953288,0.,-0.574476742810665));
#12036=CARTESIAN_POINT('Origin',(1.23586981624525,0.,-0.524595613109699));
#12037=CARTESIAN_POINT('',(1.23586981624525,1.,-0.524595613109699));
#12038=CARTESIAN_POINT('',(1.23586981624525,1.,-0.524595613109699));
#12039=CARTESIAN_POINT('',(1.23586981624525,0.,-0.524595613109699));
#12040=CARTESIAN_POINT('Origin',(0.751131960417191,0.,-0.318836600847247));
#12041=CARTESIAN_POINT('',(0.751131960417191,1.,-0.318836600847247));
#12042=CARTESIAN_POINT('Origin',(0.932067487714439,1.,-0.53812941493483));
#12043=CARTESIAN_POINT('Origin',(-1.23586981624525,0.,-0.524595613109699));
#12044=CARTESIAN_POINT('',(-0.751131960417191,1.,-0.318836600847248));
#12045=CARTESIAN_POINT('',(-0.751131960417191,0.,-0.318836600847248));
#12046=CARTESIAN_POINT('',(-1.23586981624525,1.,-0.524595613109699));
#12047=CARTESIAN_POINT('',(-1.23586981624525,1.,-0.524595613109699));
#12048=CARTESIAN_POINT('',(-1.23586981624525,-1.,-0.524595613109699));
#12049=CARTESIAN_POINT('',(-1.23586981624525,0.,-0.524595613109699));
#12050=CARTESIAN_POINT('',(-0.751131960417191,-1.,-0.318836600847248));
#12051=CARTESIAN_POINT('',(-1.23586981624525,-1.,-0.524595613109699));
#12052=CARTESIAN_POINT('',(-0.751131960417191,0.,-0.318836600847248));
#12053=CARTESIAN_POINT('Origin',(-0.751131960417191,0.,-0.318836600847248));
#12054=CARTESIAN_POINT('',(-0.737528356277993,1.,-0.34915315219239));
#12055=CARTESIAN_POINT('',(-0.737528356277993,0.,-0.34915315219239));
#12056=CARTESIAN_POINT('',(-0.751131960417191,1.,-0.318836600847248));
#12057=CARTESIAN_POINT('Origin',(-0.751131960417191,0.,-0.318836600847248));
#12058=CARTESIAN_POINT('',(-0.737528356277993,-1.,-0.34915315219239));
#12059=CARTESIAN_POINT('',(-0.751131960417191,-1.,-0.318836600847248));
#12060=CARTESIAN_POINT('',(-0.737528356277993,0.,-0.34915315219239));
#12061=CARTESIAN_POINT('Origin',(-0.737528356277993,0.,-0.34915315219239));
#12062=CARTESIAN_POINT('',(-0.722701750594522,1.,-0.378890722620143));
#12063=CARTESIAN_POINT('',(-0.722701750594522,0.,-0.378890722620143));
#12064=CARTESIAN_POINT('',(-0.737528356277993,1.,-0.34915315219239));
#12065=CARTESIAN_POINT('Origin',(-0.722701750594522,0.,-0.378890722620143));
#12066=CARTESIAN_POINT('',(-0.706676729488102,1.,-0.408));
#12067=CARTESIAN_POINT('',(-0.706676729488102,0.,-0.408));
#12068=CARTESIAN_POINT('',(-0.722701750594522,1.,-0.378890722620143));
#12069=CARTESIAN_POINT('Origin',(-0.706676729488102,0.,-0.408));
#12070=CARTESIAN_POINT('',(-0.689479866344548,1.,-0.43643271406427));
#12071=CARTESIAN_POINT('',(-0.689479866344548,0.,-0.43643271406427));
#12072=CARTESIAN_POINT('',(-0.706676729488102,1.,-0.408));
#12073=CARTESIAN_POINT('Origin',(-0.689479866344548,0.,-0.43643271406427));
#12074=CARTESIAN_POINT('',(-0.67113967774902,1.,-0.464141716451927));
#12075=CARTESIAN_POINT('',(-0.67113967774902,0.,-0.464141716451927));
#12076=CARTESIAN_POINT('',(-0.689479866344548,1.,-0.43643271406427));
#12077=CARTESIAN_POINT('Origin',(-0.67113967774902,0.,-0.464141716451927));
#12078=CARTESIAN_POINT('',(-0.651686576198591,1.,-0.491081058892072));
#12079=CARTESIAN_POINT('',(-0.651686576198591,0.,-0.491081058892072));
#12080=CARTESIAN_POINT('',(-0.67113967774902,1.,-0.464141716451927));
#12081=CARTESIAN_POINT('Origin',(-0.932067487714439,-1.,-0.53812941493483));
#12082=CARTESIAN_POINT('',(-1.0722480357895,-1.,-0.80799685008394));
#12083=CARTESIAN_POINT('',(-0.651686576198591,-1.,-0.491081058892072));
#12084=CARTESIAN_POINT('',(-0.651686576198591,-1.,-0.491081058892072));
#12085=CARTESIAN_POINT('',(-0.67113967774902,-1.,-0.464141716451927));
#12086=CARTESIAN_POINT('',(-0.67113967774902,-1.,-0.464141716451927));
#12087=CARTESIAN_POINT('',(-0.689479866344548,-1.,-0.43643271406427));
#12088=CARTESIAN_POINT('',(-0.689479866344548,-1.,-0.43643271406427));
#12089=CARTESIAN_POINT('',(-0.706676729488102,-1.,-0.408));
#12090=CARTESIAN_POINT('',(-0.706676729488102,-1.,-0.408));
#12091=CARTESIAN_POINT('',(-0.722701750594522,-1.,-0.378890722620143));
#12092=CARTESIAN_POINT('',(-0.722701750594522,-1.,-0.378890722620143));
#12093=CARTESIAN_POINT('',(-0.737528356277993,-1.,-0.34915315219239));
#12094=CARTESIAN_POINT('',(-1.21348721953288,-1.,-0.574476742810665));
#12095=CARTESIAN_POINT('',(-1.21348721953288,-1.,-0.574476742810665));
#12096=CARTESIAN_POINT('',(-1.1890923656228,-1.,-0.623405250232602));
#12097=CARTESIAN_POINT('',(-1.1890923656228,-1.,-0.623405250232602));
#12098=CARTESIAN_POINT('',(-1.16272570712099,-1.,-0.6713));
#12099=CARTESIAN_POINT('',(-1.16272570712099,-1.,-0.6713));
#12100=CARTESIAN_POINT('',(-1.13443096636543,-1.,-0.718081570959178));
#12101=CARTESIAN_POINT('',(-1.13443096636543,-1.,-0.718081570959178));
#12102=CARTESIAN_POINT('',(-1.10425506292382,-1.,-0.763672387877889));
#12103=CARTESIAN_POINT('',(-1.10425506292382,-1.,-0.763672387877889));
#12104=CARTESIAN_POINT('',(-1.0722480357895,-1.,-0.80799685008394));
#12105=CARTESIAN_POINT('Origin',(-0.67113967774902,0.,-0.464141716451927));
#12106=CARTESIAN_POINT('',(-0.67113967774902,0.,-0.464141716451927));
#12107=CARTESIAN_POINT('',(-0.651686576198591,0.,-0.491081058892072));
#12108=CARTESIAN_POINT('Origin',(-0.689479866344548,0.,-0.43643271406427));
#12109=CARTESIAN_POINT('',(-0.689479866344548,0.,-0.43643271406427));
#12110=CARTESIAN_POINT('Origin',(-0.706676729488102,0.,-0.408));
#12111=CARTESIAN_POINT('',(-0.706676729488102,0.,-0.408));
#12112=CARTESIAN_POINT('Origin',(-0.722701750594522,0.,-0.378890722620143));
#12113=CARTESIAN_POINT('',(-0.722701750594522,0.,-0.378890722620143));
#12114=CARTESIAN_POINT('Origin',(-0.737528356277993,0.,-0.34915315219239));
#12115=CARTESIAN_POINT('Origin',(-1.21348721953288,0.,-0.574476742810665));
#12116=CARTESIAN_POINT('',(-1.21348721953288,1.,-0.574476742810665));
#12117=CARTESIAN_POINT('',(-1.21348721953288,1.,-0.574476742810665));
#12118=CARTESIAN_POINT('',(-1.21348721953288,0.,-0.574476742810665));
#12119=CARTESIAN_POINT('Origin',(-1.1890923656228,0.,-0.623405250232602));
#12120=CARTESIAN_POINT('',(-1.1890923656228,1.,-0.623405250232602));
#12121=CARTESIAN_POINT('',(-1.1890923656228,1.,-0.623405250232602));
#12122=CARTESIAN_POINT('',(-1.1890923656228,0.,-0.623405250232602));
#12123=CARTESIAN_POINT('Origin',(-1.16272570712099,0.,-0.6713));
#12124=CARTESIAN_POINT('',(-1.16272570712099,1.,-0.6713));
#12125=CARTESIAN_POINT('',(-1.16272570712099,1.,-0.6713));
#12126=CARTESIAN_POINT('',(-1.16272570712099,0.,-0.6713));
#12127=CARTESIAN_POINT('Origin',(-1.13443096636543,0.,-0.718081570959178));
#12128=CARTESIAN_POINT('',(-1.13443096636543,1.,-0.718081570959178));
#12129=CARTESIAN_POINT('',(-1.13443096636543,1.,-0.718081570959178));
#12130=CARTESIAN_POINT('',(-1.13443096636543,0.,-0.718081570959178));
#12131=CARTESIAN_POINT('Origin',(-1.10425506292382,0.,-0.763672387877889));
#12132=CARTESIAN_POINT('',(-1.10425506292382,1.,-0.763672387877889));
#12133=CARTESIAN_POINT('',(-1.10425506292382,1.,-0.763672387877889));
#12134=CARTESIAN_POINT('',(-1.10425506292382,0.,-0.763672387877889));
#12135=CARTESIAN_POINT('Origin',(-1.0722480357895,0.,-0.80799685008394));
#12136=CARTESIAN_POINT('',(-1.0722480357895,1.,-0.80799685008394));
#12137=CARTESIAN_POINT('',(-1.0722480357895,1.,-0.80799685008394));
#12138=CARTESIAN_POINT('',(-1.0722480357895,0.,-0.80799685008394));
#12139=CARTESIAN_POINT('Origin',(-0.651686576198591,0.,-0.491081058892072));
#12140=CARTESIAN_POINT('',(-0.651686576198591,1.,-0.491081058892072));
#12141=CARTESIAN_POINT('Origin',(-0.932067487714439,1.,-0.53812941493483));
#12142=CARTESIAN_POINT('Origin',(0.16362178045575,0.,1.33259246319364));
#12143=CARTESIAN_POINT('',(0.0994453842185998,1.,0.809917659739319));
#12144=CARTESIAN_POINT('',(0.0994453842185998,0.,0.809917659739319));
#12145=CARTESIAN_POINT('',(0.16362178045575,1.,1.33259246319364));
#12146=CARTESIAN_POINT('',(0.16362178045575,1.,1.33259246319364));
#12147=CARTESIAN_POINT('',(0.16362178045575,-1.,1.33259246319364));
#12148=CARTESIAN_POINT('',(0.16362178045575,0.,1.33259246319364));
#12149=CARTESIAN_POINT('',(0.0994453842185998,-1.,0.809917659739319));
#12150=CARTESIAN_POINT('',(0.16362178045575,-1.,1.33259246319364));
#12151=CARTESIAN_POINT('',(0.0994453842185998,0.,0.809917659739319));
#12152=CARTESIAN_POINT('Origin',(0.0994453842185998,0.,0.809917659739319));
#12153=CARTESIAN_POINT('',(0.0663886785289718,1.,0.813294868644317));
#12154=CARTESIAN_POINT('',(0.0663886785289718,0.,0.813294868644317));
#12155=CARTESIAN_POINT('',(0.0994453842185998,1.,0.809917659739319));
#12156=CARTESIAN_POINT('Origin',(0.0994453842185998,0.,0.809917659739319));
#12157=CARTESIAN_POINT('',(0.0663886785289718,-1.,0.813294868644317));
#12158=CARTESIAN_POINT('',(0.0994453842185998,-1.,0.809917659739319));
#12159=CARTESIAN_POINT('',(0.0663886785289718,0.,0.813294868644317));
#12160=CARTESIAN_POINT('Origin',(0.0663886785289718,0.,0.813294868644317));
#12161=CARTESIAN_POINT('',(0.0332218842499737,1.,0.815323436684413));
#12162=CARTESIAN_POINT('',(0.0332218842499737,0.,0.815323436684413));
#12163=CARTESIAN_POINT('',(0.0663886785289718,1.,0.813294868644317));
#12164=CARTESIAN_POINT('Origin',(0.0332218842499737,0.,0.815323436684413));
#12165=CARTESIAN_POINT('',(-4.9960036108132E-16,1.,0.816));
#12166=CARTESIAN_POINT('',(-4.9960036108132E-16,0.,0.816));
#12167=CARTESIAN_POINT('',(0.0332218842499737,1.,0.815323436684413));
#12168=CARTESIAN_POINT('Origin',(-4.9960036108132E-16,0.,0.816));
#12169=CARTESIAN_POINT('',(-0.0332218842499747,1.,0.815323436684413));
#12170=CARTESIAN_POINT('',(-0.0332218842499747,0.,0.815323436684413));
#12171=CARTESIAN_POINT('',(-4.9960036108132E-16,1.,0.816));
#12172=CARTESIAN_POINT('Origin',(-0.0332218842499747,0.,0.815323436684413));
#12173=CARTESIAN_POINT('',(-0.0663886785289729,1.,0.813294868644317));
#12174=CARTESIAN_POINT('',(-0.0663886785289729,0.,0.813294868644317));
#12175=CARTESIAN_POINT('',(-0.0332218842499747,1.,0.815323436684413));
#12176=CARTESIAN_POINT('Origin',(-0.0663886785289729,0.,0.813294868644317));
#12177=CARTESIAN_POINT('',(-0.0994453842186008,1.,0.809917659739319));
#12178=CARTESIAN_POINT('',(-0.0994453842186008,0.,0.809917659739319));
#12179=CARTESIAN_POINT('',(-0.0663886785289729,1.,0.813294868644317));
#12180=CARTESIAN_POINT('Origin',(-6.10622663543836E-16,-1.,1.07625882986966));
#12181=CARTESIAN_POINT('',(-0.163621780455752,-1.,1.33259246319364));
#12182=CARTESIAN_POINT('',(-0.0994453842186008,-1.,0.809917659739319));
#12183=CARTESIAN_POINT('',(-0.0994453842186008,-1.,0.809917659739319));
#12184=CARTESIAN_POINT('',(-0.0663886785289729,-1.,0.813294868644317));
#12185=CARTESIAN_POINT('',(-0.0663886785289729,-1.,0.813294868644317));
#12186=CARTESIAN_POINT('',(-0.0332218842499747,-1.,0.815323436684413));
#12187=CARTESIAN_POINT('',(-0.0332218842499747,-1.,0.815323436684413));
#12188=CARTESIAN_POINT('',(-4.9960036108132E-16,-1.,0.816));
#12189=CARTESIAN_POINT('',(-4.9960036108132E-16,-1.,0.816));
#12190=CARTESIAN_POINT('',(0.0332218842499737,-1.,0.815323436684413));
#12191=CARTESIAN_POINT('',(0.0332218842499737,-1.,0.815323436684413));
#12192=CARTESIAN_POINT('',(0.0663886785289718,-1.,0.813294868644317));
#12193=CARTESIAN_POINT('',(0.109232156609066,-1.,1.33814913068855));
#12194=CARTESIAN_POINT('',(0.109232156609066,-1.,1.33814913068855));
#12195=CARTESIAN_POINT('',(0.054661399257371,-1.,1.34148682119178));
#12196=CARTESIAN_POINT('',(0.054661399257371,-1.,1.34148682119178));
#12197=CARTESIAN_POINT('',(-7.7715611723761E-16,-1.,1.3426));
#12198=CARTESIAN_POINT('',(-7.7715611723761E-16,-1.,1.3426));
#12199=CARTESIAN_POINT('',(-0.0546613992573726,-1.,1.34148682119178));
#12200=CARTESIAN_POINT('',(-0.0546613992573726,-1.,1.34148682119178));
#12201=CARTESIAN_POINT('',(-0.109232156609067,-1.,1.33814913068855));
#12202=CARTESIAN_POINT('',(-0.109232156609067,-1.,1.33814913068855));
#12203=CARTESIAN_POINT('',(-0.163621780455752,-1.,1.33259246319364));
#12204=CARTESIAN_POINT('Origin',(-0.0663886785289729,0.,0.813294868644317));
#12205=CARTESIAN_POINT('',(-0.0663886785289729,0.,0.813294868644317));
#12206=CARTESIAN_POINT('',(-0.0994453842186008,0.,0.809917659739319));
#12207=CARTESIAN_POINT('Origin',(-0.0332218842499747,0.,0.815323436684413));
#12208=CARTESIAN_POINT('',(-0.0332218842499747,0.,0.815323436684413));
#12209=CARTESIAN_POINT('Origin',(-4.9960036108132E-16,0.,0.816));
#12210=CARTESIAN_POINT('',(-4.9960036108132E-16,0.,0.816));
#12211=CARTESIAN_POINT('Origin',(0.0332218842499737,0.,0.815323436684413));
#12212=CARTESIAN_POINT('',(0.0332218842499737,0.,0.815323436684413));
#12213=CARTESIAN_POINT('Origin',(0.0663886785289718,0.,0.813294868644317));
#12214=CARTESIAN_POINT('Origin',(0.109232156609066,0.,1.33814913068855));
#12215=CARTESIAN_POINT('',(0.109232156609066,1.,1.33814913068855));
#12216=CARTESIAN_POINT('',(0.109232156609066,1.,1.33814913068855));
#12217=CARTESIAN_POINT('',(0.109232156609066,0.,1.33814913068855));
#12218=CARTESIAN_POINT('Origin',(0.054661399257371,0.,1.34148682119178));
#12219=CARTESIAN_POINT('',(0.054661399257371,1.,1.34148682119178));
#12220=CARTESIAN_POINT('',(0.054661399257371,1.,1.34148682119178));
#12221=CARTESIAN_POINT('',(0.054661399257371,0.,1.34148682119178));
#12222=CARTESIAN_POINT('Origin',(-7.7715611723761E-16,0.,1.3426));
#12223=CARTESIAN_POINT('',(-7.7715611723761E-16,1.,1.3426));
#12224=CARTESIAN_POINT('',(-7.7715611723761E-16,1.,1.3426));
#12225=CARTESIAN_POINT('',(-7.7715611723761E-16,0.,1.3426));
#12226=CARTESIAN_POINT('Origin',(-0.0546613992573726,0.,1.34148682119178));
#12227=CARTESIAN_POINT('',(-0.0546613992573726,1.,1.34148682119178));
#12228=CARTESIAN_POINT('',(-0.0546613992573726,1.,1.34148682119178));
#12229=CARTESIAN_POINT('',(-0.0546613992573726,0.,1.34148682119178));
#12230=CARTESIAN_POINT('Origin',(-0.109232156609067,0.,1.33814913068855));
#12231=CARTESIAN_POINT('',(-0.109232156609067,1.,1.33814913068855));
#12232=CARTESIAN_POINT('',(-0.109232156609067,1.,1.33814913068855));
#12233=CARTESIAN_POINT('',(-0.109232156609067,0.,1.33814913068855));
#12234=CARTESIAN_POINT('Origin',(-0.163621780455752,0.,1.33259246319364));
#12235=CARTESIAN_POINT('',(-0.163621780455752,1.,1.33259246319364));
#12236=CARTESIAN_POINT('',(-0.163621780455752,1.,1.33259246319364));
#12237=CARTESIAN_POINT('',(-0.163621780455752,0.,1.33259246319364));
#12238=CARTESIAN_POINT('Origin',(-0.0994453842186008,0.,0.809917659739319));
#12239=CARTESIAN_POINT('',(-0.0994453842186008,1.,0.809917659739319));
#12240=CARTESIAN_POINT('Origin',(-6.10622663543836E-16,1.,1.07625882986966));
#12241=CARTESIAN_POINT('',(0.,0.,0.));
#12242=CARTESIAN_POINT('',(0.,0.,0.));
#12243=CARTESIAN_POINT('',(0.,0.,0.));
#12244=CARTESIAN_POINT('',(0.,0.,0.));
#12245=CARTESIAN_POINT('Origin',(0.0721687836487032,0.,-0.125));
#12246=CARTESIAN_POINT('',(0.0721687836487032,0.,-0.125));
#12247=CARTESIAN_POINT('',(0.144337567297406,0.,0.));
#12248=CARTESIAN_POINT('',(0.117710979560879,0.,-0.0461186027918559));
#12249=CARTESIAN_POINT('',(0.0721687836487032,-0.25,-0.125));
#12250=CARTESIAN_POINT('',(0.0721687836487032,0.,-0.125));
#12251=CARTESIAN_POINT('',(0.144337567297406,-0.25,0.));
#12252=CARTESIAN_POINT('',(0.144337567297406,-0.25,0.));
#12253=CARTESIAN_POINT('',(0.144337567297406,0.,0.));
#12254=CARTESIAN_POINT('Origin',(-0.0721687836487032,0.,-0.125));
#12255=CARTESIAN_POINT('',(-0.0721687836487032,0.,-0.125));
#12256=CARTESIAN_POINT('',(0.0739156081756484,0.,-0.125));
#12257=CARTESIAN_POINT('',(-0.0721687836487032,-0.25,-0.125));
#12258=CARTESIAN_POINT('',(-0.0721687836487032,0.,-0.125));
#12259=CARTESIAN_POINT('',(0.0721687836487032,-0.25,-0.125));
#12260=CARTESIAN_POINT('Origin',(-0.144337567297406,0.,-4.16333634234434E-17));
#12261=CARTESIAN_POINT('',(-0.144337567297406,0.,-1.76762539787485E-17));
#12262=CARTESIAN_POINT('',(-0.0987953713852306,0.,-0.0788813972081442));
#12263=CARTESIAN_POINT('',(-0.144337567297406,-0.25,-2.77555756156289E-17));
#12264=CARTESIAN_POINT('',(-0.144337567297406,0.,-1.76762539787485E-17));
#12265=CARTESIAN_POINT('',(-0.0721687836487032,-0.25,-0.125));
#12266=CARTESIAN_POINT('Origin',(-0.0721687836487033,0.,0.125));
#12267=CARTESIAN_POINT('',(-0.0721687836487033,0.,0.125));
#12268=CARTESIAN_POINT('',(-0.0627109795608791,0.,0.141381397208144));
#12269=CARTESIAN_POINT('',(-0.0721687836487033,-0.25,0.125));
#12270=CARTESIAN_POINT('',(-0.0721687836487033,0.,0.125));
#12271=CARTESIAN_POINT('',(-0.144337567297406,-0.25,-1.76762539787485E-17));
#12272=CARTESIAN_POINT('Origin',(0.0721687836487032,0.,0.125));
#12273=CARTESIAN_POINT('',(0.0721687836487032,0.,0.125));
#12274=CARTESIAN_POINT('',(0.146084391824352,0.,0.125));
#12275=CARTESIAN_POINT('',(0.0721687836487032,-0.25,0.125));
#12276=CARTESIAN_POINT('',(0.0721687836487032,0.,0.125));
#12277=CARTESIAN_POINT('',(-0.0721687836487033,-0.25,0.125));
#12278=CARTESIAN_POINT('Origin',(0.144337567297406,0.,0.));
#12279=CARTESIAN_POINT('',(0.153795371385231,0.,-0.0163813972081441));
#12280=CARTESIAN_POINT('',(0.0721687836487032,-0.25,0.125));
#12281=CARTESIAN_POINT('Origin',(0.,-0.25,0.));
#12282=CARTESIAN_POINT('Origin',(0.22,0.,0.));
#12283=CARTESIAN_POINT('',(-0.22,-8.67361737988404E-18,-2.69422295812418E-17));
#12284=CARTESIAN_POINT('Origin',(0.,0.,0.));
#12285=CARTESIAN_POINT('Origin',(0.,-0.015,0.));
#12286=CARTESIAN_POINT('',(-0.24505,-0.02505,-3.00099698131059E-17));
#12287=CARTESIAN_POINT('Origin',(0.,-0.02505,0.));
#12288=CARTESIAN_POINT('',(-0.235,-0.015,-2.87791997799628E-17));
#12289=CARTESIAN_POINT('Origin',(0.,-0.3775,0.));
#12290=CARTESIAN_POINT('',(-0.24505,-0.72995,3.00099698131059E-17));
#12291=CARTESIAN_POINT('Origin',(0.,-0.72995,0.));
#12292=CARTESIAN_POINT('',(-0.24505,-0.3775,-3.00099698131059E-17));
#12293=CARTESIAN_POINT('Origin',(0.,-0.7625,0.));
#12294=CARTESIAN_POINT('',(-0.175,-0.8,-2.14313189850787E-17));
#12295=CARTESIAN_POINT('Origin',(0.,-0.8,0.));
#12296=CARTESIAN_POINT('',(-0.2125,-0.7625,-2.60237444818813E-17));
#12297=CARTESIAN_POINT('Origin',(0.,-0.8,0.));
#12298=CARTESIAN_POINT('',(0.,0.,0.));
#12299=CARTESIAN_POINT('',(0.,0.,0.));
#12300=CARTESIAN_POINT('',(0.,0.,0.));
#12301=CARTESIAN_POINT('',(0.,-9.,1.2));
#12302=CARTESIAN_POINT('',(-1.6,-9.,1.8));
#12303=CARTESIAN_POINT('',(1.6,-9.,1.8));
#12304=CARTESIAN_POINT('',(1.2,-9.,4.55));
#12305=CARTESIAN_POINT('',(0.,9.,1.2));
#12306=CARTESIAN_POINT('',(-1.6,9.,1.8));
#12307=CARTESIAN_POINT('',(1.6,9.,1.8));
#12308=CARTESIAN_POINT('',(1.2,9.,4.55));
#12309=CARTESIAN_POINT('',(0.,-11.2,3.5));
#12310=CARTESIAN_POINT('',(1.4,-10.6,3.5));
#12311=CARTESIAN_POINT('',(0.,10.,3.5));
#12312=CARTESIAN_POINT('',(1.4,10.6,3.5));
#12313=CARTESIAN_POINT('',(0.,0.,3.5));
#12314=CARTESIAN_POINT('',(0.,-1.525,4.9));
#12315=CARTESIAN_POINT('',(1.21243556529821,1.525,4.2));
#12316=UNCERTAINTY_MEASURE_WITH_UNIT(LENGTH_MEASURE(0.001),#12344,
'DISTANCE_ACCURACY_VALUE',
'Maximum model space distance between geometric entities at asserted c
onnectivities');
#12317=UNCERTAINTY_MEASURE_WITH_UNIT(LENGTH_MEASURE(0.001),#12344,
'DISTANCE_ACCURACY_VALUE',
'Maximum model space distance between geometric entities at asserted c
onnectivities');
#12318=UNCERTAINTY_MEASURE_WITH_UNIT(LENGTH_MEASURE(0.001),#12344,
'DISTANCE_ACCURACY_VALUE',
'Maximum model space distance between geometric entities at asserted c
onnectivities');
#12319=UNCERTAINTY_MEASURE_WITH_UNIT(LENGTH_MEASURE(0.001),#12344,
'DISTANCE_ACCURACY_VALUE',
'Maximum model space distance between geometric entities at asserted c
onnectivities');
#12320=UNCERTAINTY_MEASURE_WITH_UNIT(LENGTH_MEASURE(0.001),#12344,
'DISTANCE_ACCURACY_VALUE',
'Maximum model space distance between geometric entities at asserted c
onnectivities');
#12321=UNCERTAINTY_MEASURE_WITH_UNIT(LENGTH_MEASURE(0.001),#12344,
'DISTANCE_ACCURACY_VALUE',
'Maximum model space distance between geometric entities at asserted c
onnectivities');
#12322=UNCERTAINTY_MEASURE_WITH_UNIT(LENGTH_MEASURE(0.001),#12344,
'DISTANCE_ACCURACY_VALUE',
'Maximum model space distance between geometric entities at asserted c
onnectivities');
#12323=UNCERTAINTY_MEASURE_WITH_UNIT(LENGTH_MEASURE(0.001),#12344,
'DISTANCE_ACCURACY_VALUE',
'Maximum model space distance between geometric entities at asserted c
onnectivities');
#12324=UNCERTAINTY_MEASURE_WITH_UNIT(LENGTH_MEASURE(0.001),#12344,
'DISTANCE_ACCURACY_VALUE',
'Maximum model space distance between geometric entities at asserted c
onnectivities');
#12325=UNCERTAINTY_MEASURE_WITH_UNIT(LENGTH_MEASURE(0.001),#12344,
'DISTANCE_ACCURACY_VALUE',
'Maximum model space distance between geometric entities at asserted c
onnectivities');
#12326=UNCERTAINTY_MEASURE_WITH_UNIT(LENGTH_MEASURE(0.001),#12344,
'DISTANCE_ACCURACY_VALUE',
'Maximum model space distance between geometric entities at asserted c
onnectivities');
#12327=UNCERTAINTY_MEASURE_WITH_UNIT(LENGTH_MEASURE(0.001),#12344,
'DISTANCE_ACCURACY_VALUE',
'Maximum model space distance between geometric entities at asserted c
onnectivities');
#12328=UNCERTAINTY_MEASURE_WITH_UNIT(LENGTH_MEASURE(0.001),#12344,
'DISTANCE_ACCURACY_VALUE',
'Maximum model space distance between geometric entities at asserted c
onnectivities');
#12329=UNCERTAINTY_MEASURE_WITH_UNIT(LENGTH_MEASURE(0.001),#12344,
'DISTANCE_ACCURACY_VALUE',
'Maximum model space distance between geometric entities at asserted c
onnectivities');
#12330=(
GEOMETRIC_REPRESENTATION_CONTEXT(3)
GLOBAL_UNCERTAINTY_ASSIGNED_CONTEXT((#12316))
GLOBAL_UNIT_ASSIGNED_CONTEXT((#12344,#12346,#12347))
REPRESENTATION_CONTEXT('','3D')
);
#12331=(
GEOMETRIC_REPRESENTATION_CONTEXT(3)
GLOBAL_UNCERTAINTY_ASSIGNED_CONTEXT((#12317))
GLOBAL_UNIT_ASSIGNED_CONTEXT((#12344,#12346,#12347))
REPRESENTATION_CONTEXT('','3D')
);
#12332=(
GEOMETRIC_REPRESENTATION_CONTEXT(3)
GLOBAL_UNCERTAINTY_ASSIGNED_CONTEXT((#12318))
GLOBAL_UNIT_ASSIGNED_CONTEXT((#12344,#12346,#12347))
REPRESENTATION_CONTEXT('','3D')
);
#12333=(
GEOMETRIC_REPRESENTATION_CONTEXT(3)
GLOBAL_UNCERTAINTY_ASSIGNED_CONTEXT((#12319))
GLOBAL_UNIT_ASSIGNED_CONTEXT((#12344,#12346,#12347))
REPRESENTATION_CONTEXT('','3D')
);
#12334=(
GEOMETRIC_REPRESENTATION_CONTEXT(3)
GLOBAL_UNCERTAINTY_ASSIGNED_CONTEXT((#12320))
GLOBAL_UNIT_ASSIGNED_CONTEXT((#12344,#12346,#12347))
REPRESENTATION_CONTEXT('','3D')
);
#12335=(
GEOMETRIC_REPRESENTATION_CONTEXT(3)
GLOBAL_UNCERTAINTY_ASSIGNED_CONTEXT((#12321))
GLOBAL_UNIT_ASSIGNED_CONTEXT((#12344,#12346,#12347))
REPRESENTATION_CONTEXT('','3D')
);
#12336=(
GEOMETRIC_REPRESENTATION_CONTEXT(3)
GLOBAL_UNCERTAINTY_ASSIGNED_CONTEXT((#12322))
GLOBAL_UNIT_ASSIGNED_CONTEXT((#12344,#12346,#12347))
REPRESENTATION_CONTEXT('','3D')
);
#12337=(
GEOMETRIC_REPRESENTATION_CONTEXT(3)
GLOBAL_UNCERTAINTY_ASSIGNED_CONTEXT((#12323))
GLOBAL_UNIT_ASSIGNED_CONTEXT((#12344,#12346,#12347))
REPRESENTATION_CONTEXT('','3D')
);
#12338=(
GEOMETRIC_REPRESENTATION_CONTEXT(3)
GLOBAL_UNCERTAINTY_ASSIGNED_CONTEXT((#12324))
GLOBAL_UNIT_ASSIGNED_CONTEXT((#12344,#12346,#12347))
REPRESENTATION_CONTEXT('','3D')
);
#12339=(
GEOMETRIC_REPRESENTATION_CONTEXT(3)
GLOBAL_UNCERTAINTY_ASSIGNED_CONTEXT((#12325))
GLOBAL_UNIT_ASSIGNED_CONTEXT((#12344,#12346,#12347))
REPRESENTATION_CONTEXT('','3D')
);
#12340=(
GEOMETRIC_REPRESENTATION_CONTEXT(3)
GLOBAL_UNCERTAINTY_ASSIGNED_CONTEXT((#12326))
GLOBAL_UNIT_ASSIGNED_CONTEXT((#12344,#12346,#12347))
REPRESENTATION_CONTEXT('','3D')
);
#12341=(
GEOMETRIC_REPRESENTATION_CONTEXT(3)
GLOBAL_UNCERTAINTY_ASSIGNED_CONTEXT((#12327))
GLOBAL_UNIT_ASSIGNED_CONTEXT((#12344,#12346,#12347))
REPRESENTATION_CONTEXT('','3D')
);
#12342=(
GEOMETRIC_REPRESENTATION_CONTEXT(3)
GLOBAL_UNCERTAINTY_ASSIGNED_CONTEXT((#12328))
GLOBAL_UNIT_ASSIGNED_CONTEXT((#12344,#12346,#12347))
REPRESENTATION_CONTEXT('','3D')
);
#12343=(
GEOMETRIC_REPRESENTATION_CONTEXT(3)
GLOBAL_UNCERTAINTY_ASSIGNED_CONTEXT((#12329))
GLOBAL_UNIT_ASSIGNED_CONTEXT((#12344,#12346,#12347))
REPRESENTATION_CONTEXT('','3D')
);
#12344=(
LENGTH_UNIT()
NAMED_UNIT(*)
SI_UNIT(.CENTI.,.METRE.)
);
#12345=(
LENGTH_UNIT()
NAMED_UNIT(*)
SI_UNIT($,.METRE.)
);
#12346=(
NAMED_UNIT(*)
PLANE_ANGLE_UNIT()
SI_UNIT($,.RADIAN.)
);
#12347=(
NAMED_UNIT(*)
SI_UNIT($,.STERADIAN.)
SOLID_ANGLE_UNIT()
);
#12348=SHAPE_DEFINITION_REPRESENTATION(#12361,#12395);
#12349=SHAPE_DEFINITION_REPRESENTATION(#12362,#12396);
#12350=SHAPE_DEFINITION_REPRESENTATION(#12363,#12397);
#12351=SHAPE_DEFINITION_REPRESENTATION(#12364,#12398);
#12352=SHAPE_DEFINITION_REPRESENTATION(#12365,#12399);
#12353=SHAPE_DEFINITION_REPRESENTATION(#12366,#12400);
#12354=SHAPE_DEFINITION_REPRESENTATION(#12367,#12401);
#12355=SHAPE_DEFINITION_REPRESENTATION(#12368,#12402);
#12356=SHAPE_DEFINITION_REPRESENTATION(#12369,#12403);
#12357=SHAPE_DEFINITION_REPRESENTATION(#12370,#12404);
#12358=SHAPE_DEFINITION_REPRESENTATION(#12371,#12405);
#12359=SHAPE_DEFINITION_REPRESENTATION(#12372,#12406);
#12360=SHAPE_DEFINITION_REPRESENTATION(#12376,#12407);
#12361=PRODUCT_DEFINITION_SHAPE('',$,#12409);
#12362=PRODUCT_DEFINITION_SHAPE('',$,#12410);
#12363=PRODUCT_DEFINITION_SHAPE('',$,#12411);
#12364=PRODUCT_DEFINITION_SHAPE('',$,#12412);
#12365=PRODUCT_DEFINITION_SHAPE('',$,#12413);
#12366=PRODUCT_DEFINITION_SHAPE('',$,#12414);
#12367=PRODUCT_DEFINITION_SHAPE('',$,#12415);
#12368=PRODUCT_DEFINITION_SHAPE('',$,#12416);
#12369=PRODUCT_DEFINITION_SHAPE('',$,#12417);
#12370=PRODUCT_DEFINITION_SHAPE('',$,#12418);
#12371=PRODUCT_DEFINITION_SHAPE('',$,#12419);
#12372=PRODUCT_DEFINITION_SHAPE('',$,#12420);
#12373=PRODUCT_DEFINITION_SHAPE($,$,#74);
#12374=PRODUCT_DEFINITION_SHAPE($,$,#75);
#12375=PRODUCT_DEFINITION_SHAPE($,$,#76);
#12376=PRODUCT_DEFINITION_SHAPE('',$,#12421);
#12377=PRODUCT_DEFINITION_SHAPE($,$,#77);
#12378=PRODUCT_DEFINITION_SHAPE($,$,#78);
#12379=PRODUCT_DEFINITION_SHAPE($,$,#79);
#12380=PRODUCT_DEFINITION_SHAPE($,$,#80);
#12381=PRODUCT_DEFINITION_SHAPE($,$,#81);
#12382=PRODUCT_DEFINITION_SHAPE($,$,#82);
#12383=PRODUCT_DEFINITION_SHAPE($,$,#83);
#12384=PRODUCT_DEFINITION_SHAPE($,$,#84);
#12385=PRODUCT_DEFINITION_SHAPE($,$,#85);
#12386=PRODUCT_DEFINITION_SHAPE($,$,#86);
#12387=PRODUCT_DEFINITION_SHAPE($,$,#87);
#12388=PRODUCT_DEFINITION_SHAPE($,$,#88);
#12389=PRODUCT_DEFINITION_SHAPE($,$,#89);
#12390=PRODUCT_DEFINITION_SHAPE($,$,#90);
#12391=PRODUCT_DEFINITION_SHAPE($,$,#91);
#12392=PRODUCT_DEFINITION_SHAPE($,$,#92);
#12393=PRODUCT_DEFINITION_SHAPE($,$,#93);
#12394=PRODUCT_DEFINITION_SHAPE($,$,#94);
#12395=SHAPE_REPRESENTATION('',(#7482,#8026,#8027,#8028,#8029,#8030,#8031,
#8032,#8033,#8034,#8035,#8036,#8037,#8038,#8039,#8040,#8041,#8042,#8043),
#12330);
#12396=SHAPE_REPRESENTATION('',(#7483),#12331);
#12397=SHAPE_REPRESENTATION('',(#7502),#12332);
#12398=SHAPE_REPRESENTATION('',(#7508),#12333);
#12399=SHAPE_REPRESENTATION('',(#7514),#12334);
#12400=SHAPE_REPRESENTATION('',(#7552),#12335);
#12401=SHAPE_REPRESENTATION('',(#7576),#12336);
#12402=SHAPE_REPRESENTATION('',(#7602),#12337);
#12403=SHAPE_REPRESENTATION('',(#7616,#8006,#8007,#8008),#12338);
#12404=SHAPE_REPRESENTATION('',(#7617),#12339);
#12405=SHAPE_REPRESENTATION('',(#7735),#12340);
#12406=SHAPE_REPRESENTATION('',(#7853),#12341);
#12407=SHAPE_REPRESENTATION('',(#8009),#12342);
#12408=PRODUCT_DEFINITION_CONTEXT('part definition',#12449,'design');
#12409=PRODUCT_DEFINITION('PAT-026',
'PAT-026',#12422,#12408);
#12410=PRODUCT_DEFINITION('Mounting base','Mounting base',#12423,
#12408);
#12411=PRODUCT_DEFINITION('Plain shaft','Plain shaft',#12424,
#12408);
#12412=PRODUCT_DEFINITION('Plain shaft (1)','Plain shaft (1)',
#12425,#12408);
#12413=PRODUCT_DEFINITION('Relieved shaft support',
'Relieved shaft support',#12426,#12408);
#12414=PRODUCT_DEFINITION('M5x14 Cap Screw','M5x14 Cap Screw',#12427,
#12408);
#12415=PRODUCT_DEFINITION('Cap Screw - M4x16',
'Cap Screw - M4x16',#12428,#12408);
#12416=PRODUCT_DEFINITION('Shaft Collar - 12 mm Bore',
'Shaft Collar - 12 mm Bore',#12429,#12408);
#12417=PRODUCT_DEFINITION('Phased jaw coupling',
'Phased jaw coupling',#12430,#12408);
#12418=PRODUCT_DEFINITION('Hub A','Hub A',#12431,#12408);
#12419=PRODUCT_DEFINITION('Hub B','Hub B',#12432,#12408);
#12420=PRODUCT_DEFINITION('Spider','Spider',#12433,#12408);
#12421=PRODUCT_DEFINITION('Socket Set Screw - M5x8',
'Socket Set Screw - M5x8',#12434,#12408);
#12422=PRODUCT_DEFINITION_FORMATION('',$,#12451);
#12423=PRODUCT_DEFINITION_FORMATION('',$,#12452);
#12424=PRODUCT_DEFINITION_FORMATION('',$,#12453);
#12425=PRODUCT_DEFINITION_FORMATION('',$,#12454);
#12426=PRODUCT_DEFINITION_FORMATION('',$,#12455);
#12427=PRODUCT_DEFINITION_FORMATION('',$,#12456);
#12428=PRODUCT_DEFINITION_FORMATION('',$,#12457);
#12429=PRODUCT_DEFINITION_FORMATION('',$,#12458);
#12430=PRODUCT_DEFINITION_FORMATION('',$,#12459);
#12431=PRODUCT_DEFINITION_FORMATION('',$,#12460);
#12432=PRODUCT_DEFINITION_FORMATION('',$,#12461);
#12433=PRODUCT_DEFINITION_FORMATION('',$,#12462);
#12434=PRODUCT_DEFINITION_FORMATION('',$,#12463);
#12435=PRODUCT_RELATED_PRODUCT_CATEGORY(
'PAT-026',
'PAT-026',(#12451));
#12436=PRODUCT_RELATED_PRODUCT_CATEGORY('Mounting base','Mounting base',
(#12452));
#12437=PRODUCT_RELATED_PRODUCT_CATEGORY('Plain shaft','Plain shaft',(#12453));
#12438=PRODUCT_RELATED_PRODUCT_CATEGORY('Plain shaft (1)',
'Plain shaft (1)',(#12454));
#12439=PRODUCT_RELATED_PRODUCT_CATEGORY('Relieved shaft support',
'Relieved shaft support',(#12455));
#12440=PRODUCT_RELATED_PRODUCT_CATEGORY('M5x14 Cap Screw',
'M5x14 Cap Screw',(#12456));
#12441=PRODUCT_RELATED_PRODUCT_CATEGORY('Cap Screw - M4x16',
'Cap Screw - M4x16',(#12457));
#12442=PRODUCT_RELATED_PRODUCT_CATEGORY('Shaft Collar - 12 mm Bore',
'Shaft Collar - 12 mm Bore',(#12458));
#12443=PRODUCT_RELATED_PRODUCT_CATEGORY('Phased jaw coupling',
'Phased jaw coupling',(#12459));
#12444=PRODUCT_RELATED_PRODUCT_CATEGORY('Hub A','Hub A',(#12460));
#12445=PRODUCT_RELATED_PRODUCT_CATEGORY('Hub B','Hub B',(#12461));
#12446=PRODUCT_RELATED_PRODUCT_CATEGORY('Spider','Spider',(#12462));
#12447=PRODUCT_RELATED_PRODUCT_CATEGORY('Socket Set Screw - M5x8',
'Socket Set Screw - M5x8',(#12463));
#12448=APPLICATION_PROTOCOL_DEFINITION('international standard',
'automotive_design',2009,#12449);
#12449=APPLICATION_CONTEXT(
'Core Data for Automotive Mechanical Design Process');
#12450=PRODUCT_CONTEXT('part definition',#12449,'mechanical');
#12451=PRODUCT('PAT-026',
'PAT-026',
'PAT-026',(#12450));
#12452=PRODUCT('Mounting base','Mounting base',
'Mounting base',(#12450));
#12453=PRODUCT('Plain shaft','Plain shaft','Plain shaft',(#12450));
#12454=PRODUCT('Plain shaft (1)','Plain shaft (1)',
'Plain shaft (1)',(#12450));
#12455=PRODUCT('Relieved shaft support','Relieved shaft support',
'Relieved shaft support',(#12450));
#12456=PRODUCT('M5x14 Cap Screw','M5x14 Cap Screw',
'M5x14 Cap Screw',(#12450));
#12457=PRODUCT('Cap Screw - M4x16','Cap Screw - M4x16',
'Cap Screw - M4x16',(#12450));
#12458=PRODUCT('Shaft Collar - 12 mm Bore','Shaft Collar - 12 mm Bore',
'Shaft Collar - 12 mm Bore',(#12450));
#12459=PRODUCT('Phased jaw coupling','Phased jaw coupling',
'Phased jaw coupling',(#12450));
#12460=PRODUCT('Hub A','Hub A','Hub A',(#12450));
#12461=PRODUCT('Hub B','Hub B','Hub B',(#12450));
#12462=PRODUCT('Spider','Spider','Spider',(#12450));
#12463=PRODUCT('Socket Set Screw - M5x8','Socket Set Screw - M5x8',
'Socket Set Screw - M5x8',(#12450));
#12464=PRESENTATION_STYLE_ASSIGNMENT((#12470));
#12465=PRESENTATION_STYLE_ASSIGNMENT((#12471));
#12466=PRESENTATION_STYLE_ASSIGNMENT((#12472));
#12467=PRESENTATION_STYLE_ASSIGNMENT((#12473));
#12468=PRESENTATION_STYLE_ASSIGNMENT((#12474));
#12469=PRESENTATION_STYLE_ASSIGNMENT((#12475));
#12470=SURFACE_STYLE_USAGE(.BOTH.,#12476);
#12471=SURFACE_STYLE_USAGE(.BOTH.,#12477);
#12472=SURFACE_STYLE_USAGE(.BOTH.,#12478);
#12473=SURFACE_STYLE_USAGE(.BOTH.,#12479);
#12474=SURFACE_STYLE_USAGE(.BOTH.,#12480);
#12475=SURFACE_STYLE_USAGE(.BOTH.,#12481);
#12476=SURFACE_SIDE_STYLE('',(#12482));
#12477=SURFACE_SIDE_STYLE('',(#12483));
#12478=SURFACE_SIDE_STYLE('',(#12484));
#12479=SURFACE_SIDE_STYLE('',(#12485));
#12480=SURFACE_SIDE_STYLE('',(#12486));
#12481=SURFACE_SIDE_STYLE('',(#12487));
#12482=SURFACE_STYLE_FILL_AREA(#12488);
#12483=SURFACE_STYLE_FILL_AREA(#12489);
#12484=SURFACE_STYLE_FILL_AREA(#12490);
#12485=SURFACE_STYLE_FILL_AREA(#12491);
#12486=SURFACE_STYLE_FILL_AREA(#12492);
#12487=SURFACE_STYLE_FILL_AREA(#12493);
#12488=FILL_AREA_STYLE('Steel - Satin',(#12494));
#12489=FILL_AREA_STYLE('CAD Library Painted - Deep blue',(#12495));
#12490=FILL_AREA_STYLE('CAD Library Painted - Steel gray',(#12496));
#12491=FILL_AREA_STYLE('CAD Library Painted - Graphite',(#12497));
#12492=FILL_AREA_STYLE('CAD Library Painted - Off white',(#12498));
#12493=FILL_AREA_STYLE('CAD Library Painted - Engineering blue',(#12499));
#12494=FILL_AREA_STYLE_COLOUR('Steel - Satin',#12500);
#12495=FILL_AREA_STYLE_COLOUR('CAD Library Painted - Deep blue',#12501);
#12496=FILL_AREA_STYLE_COLOUR('CAD Library Painted - Steel gray',#12502);
#12497=FILL_AREA_STYLE_COLOUR('CAD Library Painted - Graphite',#12503);
#12498=FILL_AREA_STYLE_COLOUR('CAD Library Painted - Off white',#12504);
#12499=FILL_AREA_STYLE_COLOUR('CAD Library Painted - Engineering blue',
#12505);
#12500=COLOUR_RGB('Steel - Satin',0.627450980392157,0.627450980392157,0.627450980392157);
#12501=COLOUR_RGB('CAD Library Painted - Deep blue',0.0784313725490196,
0.203921568627451,0.349019607843137);
#12502=COLOUR_RGB('CAD Library Painted - Steel gray',0.592156862745098,
0.631372549019608,0.67843137254902);
#12503=COLOUR_RGB('CAD Library Painted - Graphite',0.0980392156862745,0.109803921568627,
0.125490196078431);
#12504=COLOUR_RGB('CAD Library Painted - Off white',0.909803921568627,0.901960784313726,
0.858823529411765);
#12505=COLOUR_RGB('CAD Library Painted - Engineering blue',0.12156862745098,
0.356862745098039,0.6);
#12506=COLOUR_RGB('Dark Blue',0.08,0.2,0.34);
#12507=FILL_AREA_STYLE_COLOUR('',#12506);
#12508=FILL_AREA_STYLE('',(#12507));
#12509=SURFACE_STYLE_FILL_AREA(#12508);
#12510=SURFACE_SIDE_STYLE('',(#12509));
#12511=SURFACE_STYLE_USAGE(.BOTH.,#12510);
#12512=PRESENTATION_STYLE_ASSIGNMENT((#12511));
#12513=COLOUR_RGB('Light Blue',0.38,0.62,0.78);
#12514=FILL_AREA_STYLE_COLOUR('',#12513);
#12515=FILL_AREA_STYLE('',(#12514));
#12516=SURFACE_STYLE_FILL_AREA(#12515);
#12517=SURFACE_SIDE_STYLE('',(#12516));
#12518=SURFACE_STYLE_USAGE(.BOTH.,#12517);
#12519=PRESENTATION_STYLE_ASSIGNMENT((#12518));
#12520=COLOUR_RGB('Sky Blue',0.24,0.69,0.87);
#12521=FILL_AREA_STYLE_COLOUR('',#12520);
#12522=FILL_AREA_STYLE('',(#12521));
#12523=SURFACE_STYLE_FILL_AREA(#12522);
#12524=SURFACE_SIDE_STYLE('',(#12523));
#12525=SURFACE_STYLE_USAGE(.BOTH.,#12524);
#12526=PRESENTATION_STYLE_ASSIGNMENT((#12525));
#12527=COLOUR_RGB('Grey',0.48,0.52,0.57);
#12528=FILL_AREA_STYLE_COLOUR('',#12527);
#12529=FILL_AREA_STYLE('',(#12528));
#12530=SURFACE_STYLE_FILL_AREA(#12529);
#12531=SURFACE_SIDE_STYLE('',(#12530));
#12532=SURFACE_STYLE_USAGE(.BOTH.,#12531);
#12533=PRESENTATION_STYLE_ASSIGNMENT((#12532));
#12534=COLOUR_RGB('Black',0.12,0.14,0.17);
#12535=FILL_AREA_STYLE_COLOUR('',#12534);
#12536=FILL_AREA_STYLE('',(#12535));
#12537=SURFACE_STYLE_FILL_AREA(#12536);
#12538=SURFACE_SIDE_STYLE('',(#12537));
#12539=SURFACE_STYLE_USAGE(.BOTH.,#12538);
#12540=PRESENTATION_STYLE_ASSIGNMENT((#12539));
#12541=COLOUR_RGB('Off White',0.89,0.88,0.83);
#12542=FILL_AREA_STYLE_COLOUR('',#12541);
#12543=FILL_AREA_STYLE('',(#12542));
#12544=SURFACE_STYLE_FILL_AREA(#12543);
#12545=SURFACE_SIDE_STYLE('',(#12544));
#12546=SURFACE_STYLE_USAGE(.BOTH.,#12545);
#12547=PRESENTATION_STYLE_ASSIGNMENT((#12546));
ENDSEC;
END-ISO-10303-21;
